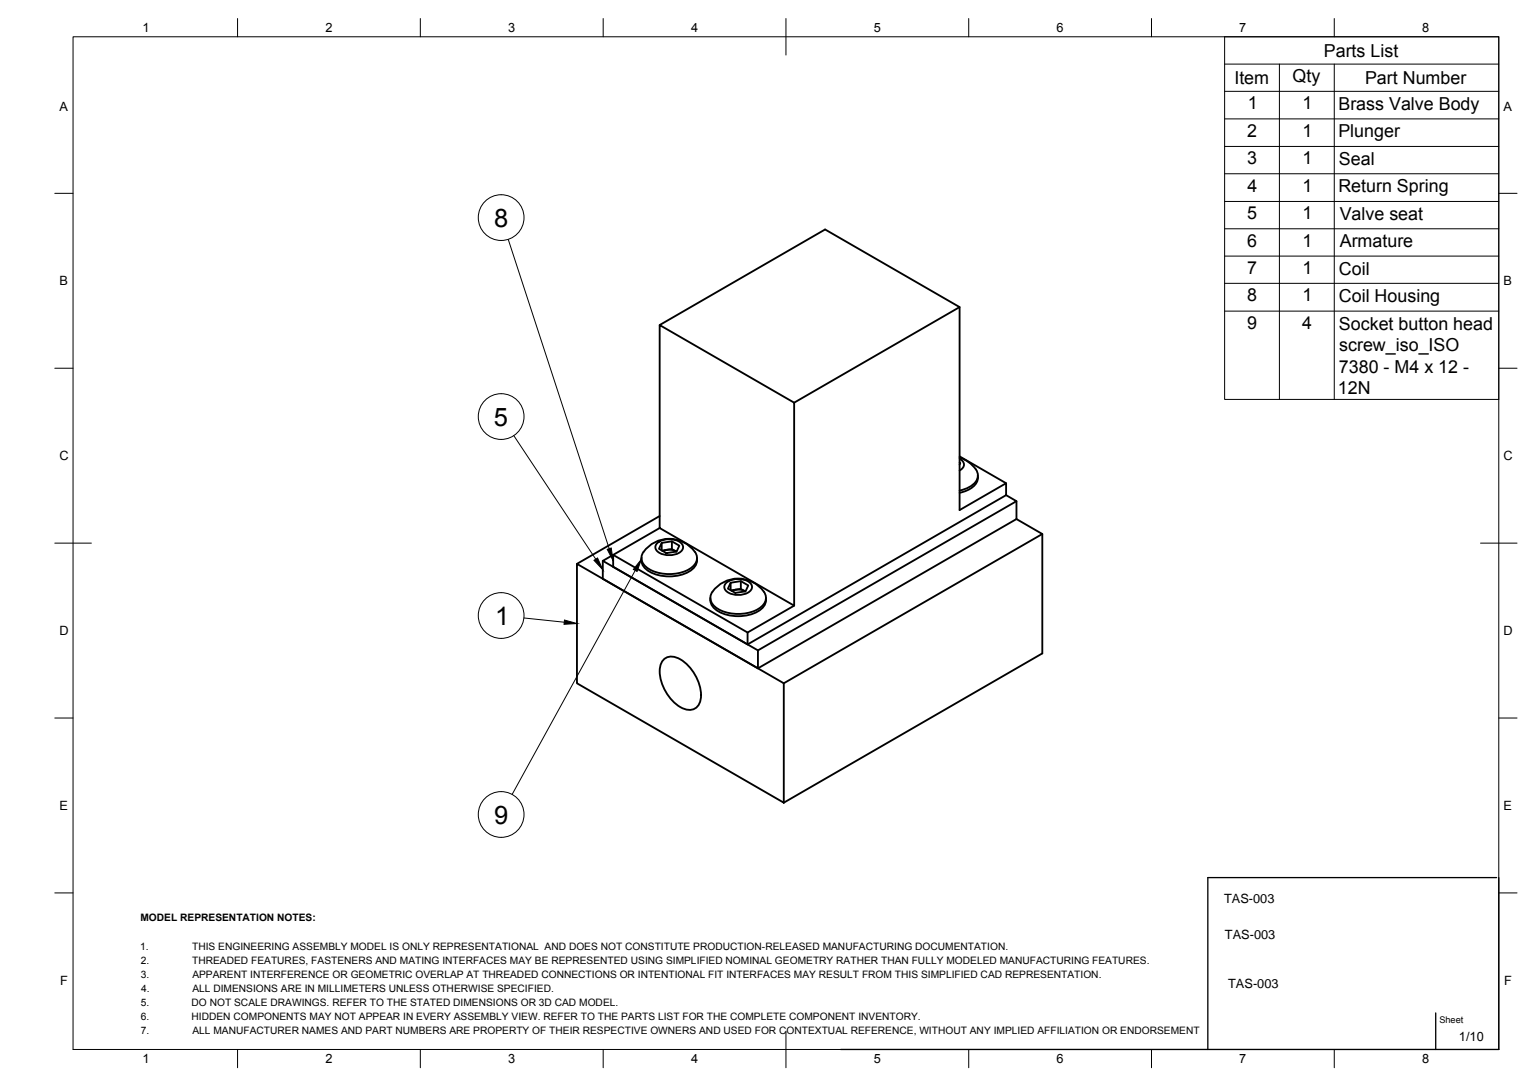
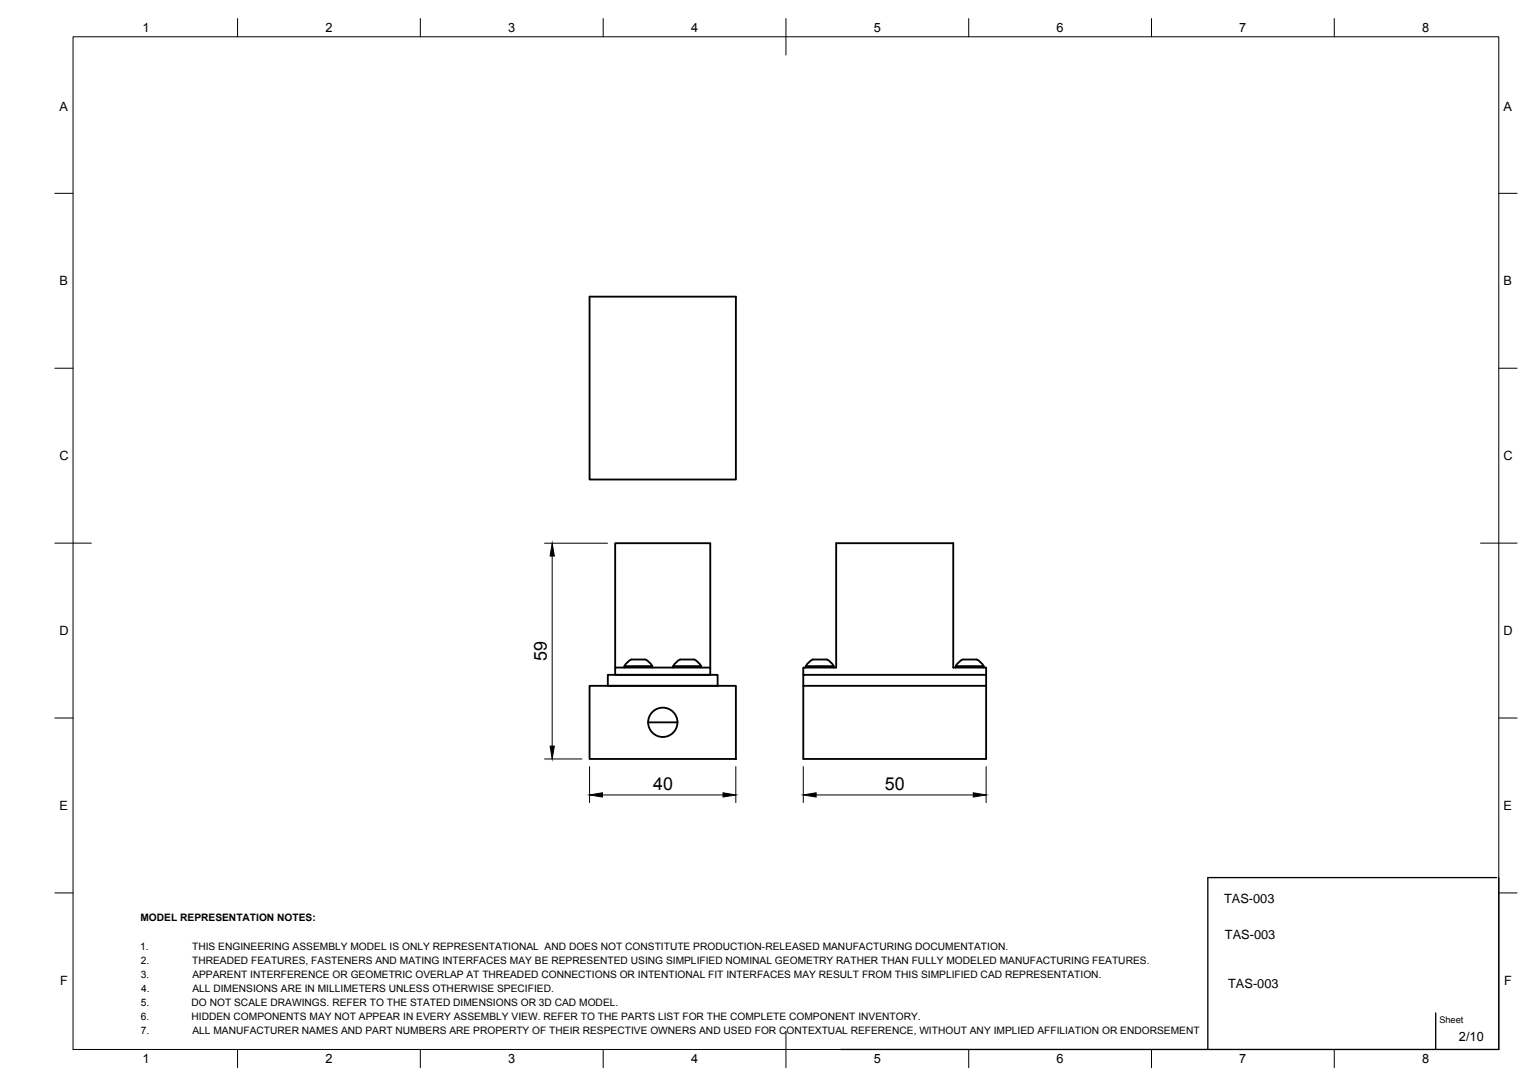
ISO-10303-21;
HEADER;
/* Generated by software containing ST-Developer
 * from STEP Tools, Inc. (www.steptools.com) 
 */

FILE_DESCRIPTION(
/* description */ ('STEP AP214'),
/* implementation_level */ '2;1');

FILE_NAME(
/* name */ 'TAS-003',
/* time_stamp */ '2026-11-04T19:43:37-08:00',
/* author */ (''),
/* organization */ (''),
/* preprocessor_version */ 'ST-DEVELOPER v20.2',
/* originating_system */ 'Autodesk Translation Framework v15.17.0.0',
/* authorisation */ '');

FILE_SCHEMA (('AUTOMOTIVE_DESIGN { 1 0 10303 214 3 1 1 }'));
ENDSEC;

DATA;
#10=MECHANICAL_DESIGN_GEOMETRIC_PRESENTATION_REPRESENTATION('',(#115,#116,
#117,#118,#119,#120,#121,#122,#123,#124,#125,#126,#127,#128,#129,#130,#131,
#132,#133,#134,#135),#7627);
#11=ITEM_DEFINED_TRANSFORMATION($,$,#2535,#2852);
#12=ITEM_DEFINED_TRANSFORMATION($,$,#2572,#2853);
#13=ITEM_DEFINED_TRANSFORMATION($,$,#2590,#2854);
#14=ITEM_DEFINED_TRANSFORMATION($,$,#2600,#2855);
#15=ITEM_DEFINED_TRANSFORMATION($,$,#2608,#2856);
#16=ITEM_DEFINED_TRANSFORMATION($,$,#2630,#2857);
#17=ITEM_DEFINED_TRANSFORMATION($,$,#2645,#2858);
#18=ITEM_DEFINED_TRANSFORMATION($,$,#2776,#2859);
#19=ITEM_DEFINED_TRANSFORMATION($,$,#2816,#2860);
#20=ITEM_DEFINED_TRANSFORMATION($,$,#2816,#2861);
#21=ITEM_DEFINED_TRANSFORMATION($,$,#2816,#2862);
#22=ITEM_DEFINED_TRANSFORMATION($,$,#2816,#2863);
#23=(
REPRESENTATION_RELATIONSHIP($,$,#7665,#7664)
REPRESENTATION_RELATIONSHIP_WITH_TRANSFORMATION(#11)
SHAPE_REPRESENTATION_RELATIONSHIP()
);
#24=(
REPRESENTATION_RELATIONSHIP($,$,#7666,#7664)
REPRESENTATION_RELATIONSHIP_WITH_TRANSFORMATION(#12)
SHAPE_REPRESENTATION_RELATIONSHIP()
);
#25=(
REPRESENTATION_RELATIONSHIP($,$,#7667,#7664)
REPRESENTATION_RELATIONSHIP_WITH_TRANSFORMATION(#13)
SHAPE_REPRESENTATION_RELATIONSHIP()
);
#26=(
REPRESENTATION_RELATIONSHIP($,$,#7668,#7664)
REPRESENTATION_RELATIONSHIP_WITH_TRANSFORMATION(#14)
SHAPE_REPRESENTATION_RELATIONSHIP()
);
#27=(
REPRESENTATION_RELATIONSHIP($,$,#7669,#7664)
REPRESENTATION_RELATIONSHIP_WITH_TRANSFORMATION(#15)
SHAPE_REPRESENTATION_RELATIONSHIP()
);
#28=(
REPRESENTATION_RELATIONSHIP($,$,#7670,#7664)
REPRESENTATION_RELATIONSHIP_WITH_TRANSFORMATION(#16)
SHAPE_REPRESENTATION_RELATIONSHIP()
);
#29=(
REPRESENTATION_RELATIONSHIP($,$,#7671,#7664)
REPRESENTATION_RELATIONSHIP_WITH_TRANSFORMATION(#17)
SHAPE_REPRESENTATION_RELATIONSHIP()
);
#30=(
REPRESENTATION_RELATIONSHIP($,$,#7672,#7664)
REPRESENTATION_RELATIONSHIP_WITH_TRANSFORMATION(#18)
SHAPE_REPRESENTATION_RELATIONSHIP()
);
#31=(
REPRESENTATION_RELATIONSHIP($,$,#7673,#7664)
REPRESENTATION_RELATIONSHIP_WITH_TRANSFORMATION(#19)
SHAPE_REPRESENTATION_RELATIONSHIP()
);
#32=(
REPRESENTATION_RELATIONSHIP($,$,#7673,#7664)
REPRESENTATION_RELATIONSHIP_WITH_TRANSFORMATION(#20)
SHAPE_REPRESENTATION_RELATIONSHIP()
);
#33=(
REPRESENTATION_RELATIONSHIP($,$,#7673,#7664)
REPRESENTATION_RELATIONSHIP_WITH_TRANSFORMATION(#21)
SHAPE_REPRESENTATION_RELATIONSHIP()
);
#34=(
REPRESENTATION_RELATIONSHIP($,$,#7673,#7664)
REPRESENTATION_RELATIONSHIP_WITH_TRANSFORMATION(#22)
SHAPE_REPRESENTATION_RELATIONSHIP()
);
#35=CONTEXT_DEPENDENT_SHAPE_REPRESENTATION(#23,#7652);
#36=CONTEXT_DEPENDENT_SHAPE_REPRESENTATION(#24,#7653);
#37=CONTEXT_DEPENDENT_SHAPE_REPRESENTATION(#25,#7654);
#38=CONTEXT_DEPENDENT_SHAPE_REPRESENTATION(#26,#7655);
#39=CONTEXT_DEPENDENT_SHAPE_REPRESENTATION(#27,#7656);
#40=CONTEXT_DEPENDENT_SHAPE_REPRESENTATION(#28,#7657);
#41=CONTEXT_DEPENDENT_SHAPE_REPRESENTATION(#29,#7658);
#42=CONTEXT_DEPENDENT_SHAPE_REPRESENTATION(#30,#7659);
#43=CONTEXT_DEPENDENT_SHAPE_REPRESENTATION(#31,#7660);
#44=CONTEXT_DEPENDENT_SHAPE_REPRESENTATION(#32,#7661);
#45=CONTEXT_DEPENDENT_SHAPE_REPRESENTATION(#33,#7662);
#46=CONTEXT_DEPENDENT_SHAPE_REPRESENTATION(#34,#7663);
#47=NEXT_ASSEMBLY_USAGE_OCCURRENCE('Brass Valve Body:1',
'Brass Valve Body:1','Brass Valve Body:1',#7675,#7676,
'Brass Valve Body:1');
#48=NEXT_ASSEMBLY_USAGE_OCCURRENCE('Plunger:1','Plunger:1','Plunger:1',
#7675,#7677,'Plunger:1');
#49=NEXT_ASSEMBLY_USAGE_OCCURRENCE('seal:1','seal:1','seal:1',#7675,#7678,
'seal:1');
#50=NEXT_ASSEMBLY_USAGE_OCCURRENCE('Return Spring:1','Return Spring:1',
'Return Spring:1',#7675,#7679,'Return Spring:1');
#51=NEXT_ASSEMBLY_USAGE_OCCURRENCE('valve seat:1','valve seat:1',
'valve seat:1',#7675,#7680,'valve seat:1');
#52=NEXT_ASSEMBLY_USAGE_OCCURRENCE('armature:1','armature:1',
'armature:1',#7675,#7681,'armature:1');
#53=NEXT_ASSEMBLY_USAGE_OCCURRENCE('coil:1','coil:1','coil:1',#7675,#7682,
'coil:1');
#54=NEXT_ASSEMBLY_USAGE_OCCURRENCE('Coil Housing:1','Coil Housing:1',
'Coil Housing:1',#7675,#7683,'Coil Housing:1');
#55=NEXT_ASSEMBLY_USAGE_OCCURRENCE(
'socket button head screw_iso_ISO 7380 - M4 x 12 - 12N:1',
'socket button head screw_iso_ISO 7380 - M4 x 12 - 12N:1',
'socket button head screw_iso_ISO 7380 - M4 x 12 - 12N:1',#7675,#7684,
'socket button head screw_iso_ISO 7380 - M4 x 12 - 12N:1');
#56=NEXT_ASSEMBLY_USAGE_OCCURRENCE(
'socket button head screw_iso_ISO 7380 - M4 x 12 - 12N:2',
'socket button head screw_iso_ISO 7380 - M4 x 12 - 12N:2',
'socket button head screw_iso_ISO 7380 - M4 x 12 - 12N:2',#7675,#7684,
'socket button head screw_iso_ISO 7380 - M4 x 12 - 12N:2');
#57=NEXT_ASSEMBLY_USAGE_OCCURRENCE(
'socket button head screw_iso_ISO 7380 - M4 x 12 - 12N:3',
'socket button head screw_iso_ISO 7380 - M4 x 12 - 12N:3',
'socket button head screw_iso_ISO 7380 - M4 x 12 - 12N:3',#7675,#7684,
'socket button head screw_iso_ISO 7380 - M4 x 12 - 12N:3');
#58=NEXT_ASSEMBLY_USAGE_OCCURRENCE(
'socket button head screw_iso_ISO 7380 - M4 x 12 - 12N:4',
'socket button head screw_iso_ISO 7380 - M4 x 12 - 12N:4',
'socket button head screw_iso_ISO 7380 - M4 x 12 - 12N:4',#7675,#7684,
'socket button head screw_iso_ISO 7380 - M4 x 12 - 12N:4');
#59=SPHERICAL_SURFACE('',#2835,4.3249693283142);
#60=TOROIDAL_SURFACE('',#2646,9.,0.999999999999999);
#61=TOROIDAL_SURFACE('',#2650,9.,0.999999999999999);
#62=TOROIDAL_SURFACE('',#2656,9.,0.999999999999999);
#63=TOROIDAL_SURFACE('',#2660,9.,0.999999999999999);
#64=TOROIDAL_SURFACE('',#2666,9.,0.999999999999999);
#65=TOROIDAL_SURFACE('',#2670,9.,0.999999999999999);
#66=TOROIDAL_SURFACE('',#2676,9.,0.999999999999999);
#67=TOROIDAL_SURFACE('',#2680,9.,0.999999999999999);
#68=TOROIDAL_SURFACE('',#2686,9.,0.999999999999999);
#69=TOROIDAL_SURFACE('',#2690,9.,0.999999999999999);
#70=TOROIDAL_SURFACE('',#2696,9.,0.999999999999999);
#71=TOROIDAL_SURFACE('',#2700,9.,0.999999999999999);
#72=TOROIDAL_SURFACE('',#2706,9.,0.999999999999999);
#73=TOROIDAL_SURFACE('',#2710,9.,0.999999999999999);
#74=TOROIDAL_SURFACE('',#2716,9.,0.999999999999999);
#75=TOROIDAL_SURFACE('',#2720,9.,0.999999999999999);
#76=TOROIDAL_SURFACE('',#2726,9.,0.999999999999999);
#77=TOROIDAL_SURFACE('',#2730,9.,0.999999999999999);
#78=TOROIDAL_SURFACE('',#2736,9.,0.999999999999999);
#79=TOROIDAL_SURFACE('',#2740,9.,0.999999999999999);
#80=TOROIDAL_SURFACE('',#2746,9.,0.999999999999999);
#81=TOROIDAL_SURFACE('',#2750,9.,0.999999999999999);
#82=TOROIDAL_SURFACE('',#2756,9.,0.999999999999999);
#83=TOROIDAL_SURFACE('',#2760,9.,0.999999999999999);
#84=TOROIDAL_SURFACE('',#2766,9.,0.999999999999999);
#85=TOROIDAL_SURFACE('',#2770,9.,0.999999999999999);
#86=TOROIDAL_SURFACE('',#2777,2.2,0.2);
#87=TOROIDAL_SURFACE('',#2781,2.2,0.2);
#88=TOROIDAL_SURFACE('',#2785,2.2,0.2);
#89=TOROIDAL_SURFACE('',#2789,2.2,0.2);
#90=TOROIDAL_SURFACE('',#2824,2.2,0.2);
#91=(
BOUNDED_CURVE()
B_SPLINE_CURVE(2,(#5252,#5253,#5254,#5255,#5256,#5257,#5258,#5259,#5260,
#5261,#5262,#5263,#5264,#5265,#5266,#5267,#5268,#5269,#5270,#5271,#5272,
#5273,#5274,#5275,#5276,#5277,#5278,#5279,#5280,#5281,#5282,#5283,#5284,
#5285,#5286,#5287,#5288,#5289,#5290,#5291,#5292,#5293,#5294,#5295,#5296,
#5297,#5298,#5299,#5300,#5301,#5302,#5303,#5304,#5305,#5306,#5307,#5308,
#5309,#5310,#5311,#5312,#5313,#5314,#5315,#5316,#5317,#5318,#5319,#5320,
#5321,#5322,#5323,#5324,#5325,#5326,#5327,#5328,#5329,#5330,#5331,#5332,
#5333,#5334,#5335,#5336,#5337,#5338,#5339,#5340,#5341,#5342,#5343,#5344,
#5345,#5346,#5347,#5348,#5349,#5350,#5351,#5352,#5353,#5354,#5355,#5356,
#5357,#5358,#5359,#5360,#5361,#5362,#5363,#5364,#5365,#5366,#5367,#5368,
#5369,#5370,#5371,#5372,#5373,#5374,#5375,#5376,#5377,#5378,#5379,#5380,
#5381,#5382,#5383,#5384,#5385,#5386,#5387,#5388,#5389,#5390,#5391,#5392,
#5393,#5394,#5395,#5396,#5397,#5398,#5399,#5400,#5401,#5402,#5403,#5404,
#5405,#5406,#5407,#5408,#5409,#5410,#5411,#5412,#5413,#5414,#5415,#5416,
#5417,#5418,#5419,#5420,#5421,#5422,#5423,#5424,#5425,#5426,#5427,#5428,
#5429,#5430,#5431,#5432,#5433,#5434,#5435,#5436,#5437,#5438,#5439,#5440,
#5441,#5442,#5443,#5444,#5445,#5446,#5447,#5448,#5449,#5450),
 .UNSPECIFIED.,.F.,.F.)
B_SPLINE_CURVE_WITH_KNOTS((3,2,2,2,2,2,2,2,2,2,2,2,2,2,2,2,2,2,2,2,2,2,
2,2,2,2,2,2,2,2,2,2,2,2,2,2,2,2,2,2,2,2,2,2,2,2,2,2,2,2,2,2,2,2,2,2,2,2,
2,2,2,2,2,2,2,2,2,2,2,2,2,2,2,2,2,2,2,2,2,2,2,2,2,2,2,2,2,2,2,2,2,2,2,2,
2,2,2,2,2,3),(0.0198656835159411,0.02,0.03,0.04,0.05,0.06,0.07,0.08,0.09,
0.1,0.11,0.12,0.13,0.14,0.15,0.16,0.17,0.18,0.19,0.2,0.21,0.22,0.23,0.24,
0.25,0.26,0.27,0.28,0.29,0.3,0.31,0.32,0.33,0.34,0.35,0.36,0.37,0.38,0.39,
0.4,0.41,0.42,0.43,0.44,0.45,0.46,0.47,0.48,0.49,0.5,0.51,0.52,0.53,0.54,
0.55,0.56,0.57,0.58,0.59,0.6,0.61,0.62,0.63,0.64,0.65,0.66,0.67,0.68,0.69,
0.7,0.71,0.72,0.73,0.74,0.75,0.76,0.77,0.78,0.79,0.8,0.81,0.82,0.83,0.84,
0.85,0.86,0.87,0.88,0.89,0.9,0.91,0.92,0.93,0.94,0.95,0.96,0.97,0.98,0.99,
1.),.UNSPECIFIED.)
CURVE()
GEOMETRIC_REPRESENTATION_ITEM()
RATIONAL_B_SPLINE_CURVE((0.998702876377649,0.999342608335117,1.,0.951056516295154,
1.,0.951056516295154,1.,0.951056516295154,1.,0.951056516295154,1.,0.951056516295154,
1.,0.951056516295154,1.,0.951056516295154,1.,0.951056516295154,1.,0.951056516295154,
1.,0.951056516295154,1.,0.951056516295154,1.,0.951056516295154,1.,0.951056516295154,
1.,0.951056516295154,1.,0.951056516295154,1.,0.951056516295154,1.,0.951056516295154,
1.,0.951056516295154,1.,0.951056516295154,1.,0.951056516295154,1.,0.951056516295154,
1.,0.951056516295154,1.,0.951056516295154,1.,0.951056516295154,1.,0.951056516295154,
1.,0.951056516295154,1.,0.951056516295154,1.,0.951056516295154,1.,0.951056516295154,
1.,0.951056516295154,1.,0.951056516295154,1.,0.951056516295154,1.,0.951056516295154,
1.,0.951056516295154,1.,0.951056516295154,1.,0.951056516295154,1.,0.951056516295154,
1.,0.951056516295154,1.,0.951056516295154,1.,0.951056516295154,1.,0.951056516295154,
1.,0.951056516295154,1.,0.951056516295154,1.,0.951056516295154,1.,0.951056516295154,
1.,0.951056516295154,1.,0.951056516295154,1.,0.951056516295154,1.,0.951056516295154,
1.,0.951056516295154,1.,0.951056516295154,1.,0.951056516295154,1.,0.951056516295154,
1.,0.951056516295154,1.,0.951056516295154,1.,0.951056516295154,1.,0.951056516295154,
1.,0.951056516295154,1.,0.951056516295154,1.,0.951056516295154,1.,0.951056516295154,
1.,0.951056516295154,1.,0.951056516295154,1.,0.951056516295154,1.,0.951056516295154,
1.,0.951056516295154,1.,0.951056516295154,1.,0.951056516295154,1.,0.951056516295154,
1.,0.951056516295154,1.,0.951056516295154,1.,0.951056516295154,1.,0.951056516295154,
1.,0.951056516295154,1.,0.951056516295154,1.,0.951056516295154,1.,0.951056516295154,
1.,0.951056516295154,1.,0.951056516295154,1.,0.951056516295154,1.,0.951056516295154,
1.,0.951056516295154,1.,0.951056516295154,1.,0.951056516295154,1.,0.951056516295154,
1.,0.951056516295154,1.,0.951056516295154,1.,0.951056516295154,1.,0.951056516295154,
1.,0.951056516295154,1.,0.951056516295154,1.,0.951056516295154,1.,0.951056516295154,
1.,0.951056516295154,1.,0.951056516295154,1.,0.951056516295154,1.,0.951056516295154,
1.,0.951056516295154,1.))
REPRESENTATION_ITEM('')
);
#92=(
BOUNDED_CURVE()
B_SPLINE_CURVE(2,(#5454,#5455,#5456,#5457,#5458,#5459,#5460,#5461,#5462,
#5463,#5464,#5465,#5466,#5467,#5468,#5469,#5470,#5471,#5472,#5473,#5474,
#5475,#5476,#5477,#5478,#5479,#5480,#5481,#5482,#5483,#5484,#5485,#5486,
#5487,#5488,#5489,#5490,#5491,#5492,#5493,#5494,#5495,#5496,#5497,#5498,
#5499,#5500,#5501,#5502,#5503,#5504,#5505,#5506,#5507,#5508,#5509,#5510,
#5511,#5512,#5513,#5514,#5515,#5516,#5517,#5518,#5519,#5520,#5521,#5522,
#5523,#5524,#5525,#5526,#5527,#5528,#5529,#5530,#5531,#5532,#5533,#5534,
#5535,#5536,#5537,#5538,#5539,#5540,#5541,#5542,#5543,#5544,#5545,#5546,
#5547,#5548,#5549,#5550,#5551,#5552,#5553,#5554,#5555,#5556,#5557,#5558,
#5559,#5560,#5561,#5562,#5563,#5564,#5565,#5566,#5567,#5568,#5569,#5570,
#5571,#5572,#5573,#5574,#5575,#5576,#5577,#5578,#5579,#5580,#5581,#5582,
#5583,#5584,#5585,#5586,#5587,#5588,#5589,#5590,#5591,#5592,#5593,#5594,
#5595,#5596,#5597,#5598,#5599,#5600,#5601,#5602,#5603,#5604,#5605,#5606,
#5607,#5608,#5609,#5610,#5611,#5612,#5613,#5614,#5615,#5616,#5617,#5618,
#5619,#5620,#5621,#5622,#5623,#5624,#5625,#5626,#5627,#5628,#5629,#5630,
#5631,#5632,#5633,#5634,#5635,#5636,#5637,#5638,#5639,#5640,#5641,#5642,
#5643,#5644,#5645,#5646,#5647,#5648,#5649,#5650,#5651,#5652,#5653,#5654),
 .UNSPECIFIED.,.F.,.F.)
B_SPLINE_CURVE_WITH_KNOTS((3,2,2,2,2,2,2,2,2,2,2,2,2,2,2,2,2,2,2,2,2,2,
2,2,2,2,2,2,2,2,2,2,2,2,2,2,2,2,2,2,2,2,2,2,2,2,2,2,2,2,2,2,2,2,2,2,2,2,
2,2,2,2,2,2,2,2,2,2,2,2,2,2,2,2,2,2,2,2,2,2,2,2,2,2,2,2,2,2,2,2,2,2,2,2,
2,2,2,2,2,2,3),(0.,0.01,0.02,0.03,0.04,0.05,0.06,0.07,0.08,0.09,0.1,0.11,
0.12,0.13,0.14,0.15,0.16,0.17,0.18,0.19,0.2,0.21,0.22,0.23,0.24,0.25,0.26,
0.27,0.28,0.29,0.3,0.31,0.32,0.33,0.34,0.35,0.36,0.37,0.38,0.39,0.4,0.41,
0.42,0.43,0.44,0.45,0.46,0.47,0.48,0.49,0.5,0.51,0.52,0.53,0.54,0.55,0.56,
0.57,0.58,0.59,0.6,0.61,0.62,0.63,0.64,0.65,0.66,0.67,0.68,0.69,0.7,0.71,
0.72,0.73,0.74,0.75,0.76,0.77,0.78,0.79,0.8,0.81,0.82,0.83,0.84,0.85,0.86,
0.87,0.88,0.89,0.9,0.91,0.92,0.93,0.94,0.95,0.96,0.97,0.98,0.99,1.),
 .UNSPECIFIED.)
CURVE()
GEOMETRIC_REPRESENTATION_ITEM()
RATIONAL_B_SPLINE_CURVE((1.,0.951056516295154,1.,0.951056516295154,1.,0.951056516295154,
1.,0.951056516295154,1.,0.951056516295154,1.,0.951056516295154,1.,0.951056516295154,
1.,0.951056516295154,1.,0.951056516295154,1.,0.951056516295154,1.,0.951056516295154,
1.,0.951056516295154,1.,0.951056516295154,1.,0.951056516295154,1.,0.951056516295154,
1.,0.951056516295154,1.,0.951056516295154,1.,0.951056516295154,1.,0.951056516295154,
1.,0.951056516295154,1.,0.951056516295154,1.,0.951056516295154,1.,0.951056516295154,
1.,0.951056516295154,1.,0.951056516295154,1.,0.951056516295154,1.,0.951056516295154,
1.,0.951056516295154,1.,0.951056516295154,1.,0.951056516295154,1.,0.951056516295154,
1.,0.951056516295154,1.,0.951056516295154,1.,0.951056516295154,1.,0.951056516295154,
1.,0.951056516295154,1.,0.951056516295154,1.,0.951056516295154,1.,0.951056516295154,
1.,0.951056516295154,1.,0.951056516295154,1.,0.951056516295154,1.,0.951056516295154,
1.,0.951056516295154,1.,0.951056516295154,1.,0.951056516295154,1.,0.951056516295154,
1.,0.951056516295154,1.,0.951056516295154,1.,0.951056516295154,1.,0.951056516295154,
1.,0.951056516295154,1.,0.951056516295154,1.,0.951056516295154,1.,0.951056516295154,
1.,0.951056516295154,1.,0.951056516295154,1.,0.951056516295154,1.,0.951056516295154,
1.,0.951056516295154,1.,0.951056516295154,1.,0.951056516295154,1.,0.951056516295154,
1.,0.951056516295154,1.,0.951056516295154,1.,0.951056516295154,1.,0.951056516295154,
1.,0.951056516295154,1.,0.951056516295154,1.,0.951056516295154,1.,0.951056516295154,
1.,0.951056516295154,1.,0.951056516295154,1.,0.951056516295154,1.,0.951056516295154,
1.,0.951056516295154,1.,0.951056516295154,1.,0.951056516295154,1.,0.951056516295154,
1.,0.951056516295154,1.,0.951056516295154,1.,0.951056516295154,1.,0.951056516295154,
1.,0.951056516295154,1.,0.951056516295154,1.,0.951056516295154,1.,0.951056516295154,
1.,0.951056516295154,1.,0.951056516295154,1.,0.951056516295154,1.,0.951056516295154,
1.,0.951056516295154,1.,0.951056516295154,1.,0.951056516295154,1.,0.951056516295154,
1.,0.951056516295154,1.,0.951056516295154,1.,0.951056516295154,1.,0.951056516295154,
1.,0.951056516295154,1.))
REPRESENTATION_ITEM('')
);
#93=B_SPLINE_CURVE_WITH_KNOTS('',3,(#5233,#5234,#5235,#5236,#5237,#5238,
#5239,#5240,#5241,#5242,#5243,#5244,#5245,#5246,#5247,#5248,#5249,#5250),
 .UNSPECIFIED.,.F.,.F.,(4,2,2,2,2,2,2,2,4),(1.00001181076875E-6,0.00157652680691075,
0.00330831465659758,0.00743558655671621,0.0176553842502255,0.0434588790338826,
0.0717527150596022,0.0885002828939342,0.104340792550165),.UNSPECIFIED.);
#94=B_SPLINE_CURVE_WITH_KNOTS('',3,(#7069,#7070,#7071,#7072,#7073,#7074,
#7075,#7076,#7077,#7078,#7079,#7080,#7081,#7082,#7083,#7084,#7085,#7086),
 .UNSPECIFIED.,.F.,.F.,(4,2,2,2,2,2,2,2,4),(0.,0.132188814767311,0.250674887289718,
0.391272166110131,0.552836235371939,0.655950520994649,0.689957274574409,
0.701859173270786,0.711834218003037),.UNSPECIFIED.);
#95=(
BOUNDED_SURFACE()
B_SPLINE_SURFACE(3,2,((#3824,#3825,#3826,#3827,#3828,#3829,#3830,#3831,
#3832,#3833,#3834,#3835,#3836,#3837,#3838,#3839,#3840,#3841,#3842,#3843,
#3844,#3845,#3846,#3847,#3848,#3849,#3850,#3851,#3852,#3853,#3854,#3855,
#3856,#3857,#3858,#3859,#3860,#3861,#3862,#3863,#3864,#3865,#3866,#3867,
#3868,#3869,#3870,#3871,#3872,#3873,#3874,#3875,#3876,#3877,#3878,#3879,
#3880,#3881,#3882,#3883,#3884,#3885,#3886,#3887,#3888,#3889,#3890,#3891,
#3892,#3893,#3894,#3895,#3896,#3897,#3898,#3899,#3900,#3901,#3902,#3903,
#3904,#3905,#3906,#3907,#3908,#3909,#3910,#3911,#3912,#3913,#3914,#3915,
#3916,#3917,#3918,#3919,#3920,#3921,#3922,#3923,#3924,#3925,#3926,#3927,
#3928,#3929,#3930,#3931,#3932,#3933,#3934,#3935,#3936,#3937,#3938,#3939,
#3940,#3941,#3942,#3943,#3944,#3945,#3946,#3947,#3948,#3949,#3950,#3951,
#3952,#3953,#3954,#3955,#3956,#3957,#3958,#3959,#3960,#3961,#3962,#3963,
#3964,#3965,#3966,#3967,#3968,#3969,#3970,#3971,#3972,#3973,#3974,#3975,
#3976,#3977,#3978,#3979,#3980,#3981,#3982,#3983,#3984,#3985,#3986,#3987,
#3988,#3989,#3990,#3991,#3992,#3993,#3994,#3995,#3996,#3997,#3998,#3999,
#4000,#4001,#4002,#4003,#4004,#4005,#4006,#4007,#4008,#4009,#4010,#4011,
#4012,#4013,#4014,#4015,#4016,#4017,#4018,#4019,#4020,#4021,#4022,#4023,
#4024),(#4025,#4026,#4027,#4028,#4029,#4030,#4031,#4032,#4033,#4034,#4035,
#4036,#4037,#4038,#4039,#4040,#4041,#4042,#4043,#4044,#4045,#4046,#4047,
#4048,#4049,#4050,#4051,#4052,#4053,#4054,#4055,#4056,#4057,#4058,#4059,
#4060,#4061,#4062,#4063,#4064,#4065,#4066,#4067,#4068,#4069,#4070,#4071,
#4072,#4073,#4074,#4075,#4076,#4077,#4078,#4079,#4080,#4081,#4082,#4083,
#4084,#4085,#4086,#4087,#4088,#4089,#4090,#4091,#4092,#4093,#4094,#4095,
#4096,#4097,#4098,#4099,#4100,#4101,#4102,#4103,#4104,#4105,#4106,#4107,
#4108,#4109,#4110,#4111,#4112,#4113,#4114,#4115,#4116,#4117,#4118,#4119,
#4120,#4121,#4122,#4123,#4124,#4125,#4126,#4127,#4128,#4129,#4130,#4131,
#4132,#4133,#4134,#4135,#4136,#4137,#4138,#4139,#4140,#4141,#4142,#4143,
#4144,#4145,#4146,#4147,#4148,#4149,#4150,#4151,#4152,#4153,#4154,#4155,
#4156,#4157,#4158,#4159,#4160,#4161,#4162,#4163,#4164,#4165,#4166,#4167,
#4168,#4169,#4170,#4171,#4172,#4173,#4174,#4175,#4176,#4177,#4178,#4179,
#4180,#4181,#4182,#4183,#4184,#4185,#4186,#4187,#4188,#4189,#4190,#4191,
#4192,#4193,#4194,#4195,#4196,#4197,#4198,#4199,#4200,#4201,#4202,#4203,
#4204,#4205,#4206,#4207,#4208,#4209,#4210,#4211,#4212,#4213,#4214,#4215,
#4216,#4217,#4218,#4219,#4220,#4221,#4222,#4223,#4224,#4225),(#4226,#4227,
#4228,#4229,#4230,#4231,#4232,#4233,#4234,#4235,#4236,#4237,#4238,#4239,
#4240,#4241,#4242,#4243,#4244,#4245,#4246,#4247,#4248,#4249,#4250,#4251,
#4252,#4253,#4254,#4255,#4256,#4257,#4258,#4259,#4260,#4261,#4262,#4263,
#4264,#4265,#4266,#4267,#4268,#4269,#4270,#4271,#4272,#4273,#4274,#4275,
#4276,#4277,#4278,#4279,#4280,#4281,#4282,#4283,#4284,#4285,#4286,#4287,
#4288,#4289,#4290,#4291,#4292,#4293,#4294,#4295,#4296,#4297,#4298,#4299,
#4300,#4301,#4302,#4303,#4304,#4305,#4306,#4307,#4308,#4309,#4310,#4311,
#4312,#4313,#4314,#4315,#4316,#4317,#4318,#4319,#4320,#4321,#4322,#4323,
#4324,#4325,#4326,#4327,#4328,#4329,#4330,#4331,#4332,#4333,#4334,#4335,
#4336,#4337,#4338,#4339,#4340,#4341,#4342,#4343,#4344,#4345,#4346,#4347,
#4348,#4349,#4350,#4351,#4352,#4353,#4354,#4355,#4356,#4357,#4358,#4359,
#4360,#4361,#4362,#4363,#4364,#4365,#4366,#4367,#4368,#4369,#4370,#4371,
#4372,#4373,#4374,#4375,#4376,#4377,#4378,#4379,#4380,#4381,#4382,#4383,
#4384,#4385,#4386,#4387,#4388,#4389,#4390,#4391,#4392,#4393,#4394,#4395,
#4396,#4397,#4398,#4399,#4400,#4401,#4402,#4403,#4404,#4405,#4406,#4407,
#4408,#4409,#4410,#4411,#4412,#4413,#4414,#4415,#4416,#4417,#4418,#4419,
#4420,#4421,#4422,#4423,#4424,#4425,#4426),(#4427,#4428,#4429,#4430,#4431,
#4432,#4433,#4434,#4435,#4436,#4437,#4438,#4439,#4440,#4441,#4442,#4443,
#4444,#4445,#4446,#4447,#4448,#4449,#4450,#4451,#4452,#4453,#4454,#4455,
#4456,#4457,#4458,#4459,#4460,#4461,#4462,#4463,#4464,#4465,#4466,#4467,
#4468,#4469,#4470,#4471,#4472,#4473,#4474,#4475,#4476,#4477,#4478,#4479,
#4480,#4481,#4482,#4483,#4484,#4485,#4486,#4487,#4488,#4489,#4490,#4491,
#4492,#4493,#4494,#4495,#4496,#4497,#4498,#4499,#4500,#4501,#4502,#4503,
#4504,#4505,#4506,#4507,#4508,#4509,#4510,#4511,#4512,#4513,#4514,#4515,
#4516,#4517,#4518,#4519,#4520,#4521,#4522,#4523,#4524,#4525,#4526,#4527,
#4528,#4529,#4530,#4531,#4532,#4533,#4534,#4535,#4536,#4537,#4538,#4539,
#4540,#4541,#4542,#4543,#4544,#4545,#4546,#4547,#4548,#4549,#4550,#4551,
#4552,#4553,#4554,#4555,#4556,#4557,#4558,#4559,#4560,#4561,#4562,#4563,
#4564,#4565,#4566,#4567,#4568,#4569,#4570,#4571,#4572,#4573,#4574,#4575,
#4576,#4577,#4578,#4579,#4580,#4581,#4582,#4583,#4584,#4585,#4586,#4587,
#4588,#4589,#4590,#4591,#4592,#4593,#4594,#4595,#4596,#4597,#4598,#4599,
#4600,#4601,#4602,#4603,#4604,#4605,#4606,#4607,#4608,#4609,#4610,#4611,
#4612,#4613,#4614,#4615,#4616,#4617,#4618,#4619,#4620,#4621,#4622,#4623,
#4624,#4625,#4626,#4627),(#4628,#4629,#4630,#4631,#4632,#4633,#4634,#4635,
#4636,#4637,#4638,#4639,#4640,#4641,#4642,#4643,#4644,#4645,#4646,#4647,
#4648,#4649,#4650,#4651,#4652,#4653,#4654,#4655,#4656,#4657,#4658,#4659,
#4660,#4661,#4662,#4663,#4664,#4665,#4666,#4667,#4668,#4669,#4670,#4671,
#4672,#4673,#4674,#4675,#4676,#4677,#4678,#4679,#4680,#4681,#4682,#4683,
#4684,#4685,#4686,#4687,#4688,#4689,#4690,#4691,#4692,#4693,#4694,#4695,
#4696,#4697,#4698,#4699,#4700,#4701,#4702,#4703,#4704,#4705,#4706,#4707,
#4708,#4709,#4710,#4711,#4712,#4713,#4714,#4715,#4716,#4717,#4718,#4719,
#4720,#4721,#4722,#4723,#4724,#4725,#4726,#4727,#4728,#4729,#4730,#4731,
#4732,#4733,#4734,#4735,#4736,#4737,#4738,#4739,#4740,#4741,#4742,#4743,
#4744,#4745,#4746,#4747,#4748,#4749,#4750,#4751,#4752,#4753,#4754,#4755,
#4756,#4757,#4758,#4759,#4760,#4761,#4762,#4763,#4764,#4765,#4766,#4767,
#4768,#4769,#4770,#4771,#4772,#4773,#4774,#4775,#4776,#4777,#4778,#4779,
#4780,#4781,#4782,#4783,#4784,#4785,#4786,#4787,#4788,#4789,#4790,#4791,
#4792,#4793,#4794,#4795,#4796,#4797,#4798,#4799,#4800,#4801,#4802,#4803,
#4804,#4805,#4806,#4807,#4808,#4809,#4810,#4811,#4812,#4813,#4814,#4815,
#4816,#4817,#4818,#4819,#4820,#4821,#4822,#4823,#4824,#4825,#4826,#4827,
#4828),(#4829,#4830,#4831,#4832,#4833,#4834,#4835,#4836,#4837,#4838,#4839,
#4840,#4841,#4842,#4843,#4844,#4845,#4846,#4847,#4848,#4849,#4850,#4851,
#4852,#4853,#4854,#4855,#4856,#4857,#4858,#4859,#4860,#4861,#4862,#4863,
#4864,#4865,#4866,#4867,#4868,#4869,#4870,#4871,#4872,#4873,#4874,#4875,
#4876,#4877,#4878,#4879,#4880,#4881,#4882,#4883,#4884,#4885,#4886,#4887,
#4888,#4889,#4890,#4891,#4892,#4893,#4894,#4895,#4896,#4897,#4898,#4899,
#4900,#4901,#4902,#4903,#4904,#4905,#4906,#4907,#4908,#4909,#4910,#4911,
#4912,#4913,#4914,#4915,#4916,#4917,#4918,#4919,#4920,#4921,#4922,#4923,
#4924,#4925,#4926,#4927,#4928,#4929,#4930,#4931,#4932,#4933,#4934,#4935,
#4936,#4937,#4938,#4939,#4940,#4941,#4942,#4943,#4944,#4945,#4946,#4947,
#4948,#4949,#4950,#4951,#4952,#4953,#4954,#4955,#4956,#4957,#4958,#4959,
#4960,#4961,#4962,#4963,#4964,#4965,#4966,#4967,#4968,#4969,#4970,#4971,
#4972,#4973,#4974,#4975,#4976,#4977,#4978,#4979,#4980,#4981,#4982,#4983,
#4984,#4985,#4986,#4987,#4988,#4989,#4990,#4991,#4992,#4993,#4994,#4995,
#4996,#4997,#4998,#4999,#5000,#5001,#5002,#5003,#5004,#5005,#5006,#5007,
#5008,#5009,#5010,#5011,#5012,#5013,#5014,#5015,#5016,#5017,#5018,#5019,
#5020,#5021,#5022,#5023,#5024,#5025,#5026,#5027,#5028,#5029),(#5030,#5031,
#5032,#5033,#5034,#5035,#5036,#5037,#5038,#5039,#5040,#5041,#5042,#5043,
#5044,#5045,#5046,#5047,#5048,#5049,#5050,#5051,#5052,#5053,#5054,#5055,
#5056,#5057,#5058,#5059,#5060,#5061,#5062,#5063,#5064,#5065,#5066,#5067,
#5068,#5069,#5070,#5071,#5072,#5073,#5074,#5075,#5076,#5077,#5078,#5079,
#5080,#5081,#5082,#5083,#5084,#5085,#5086,#5087,#5088,#5089,#5090,#5091,
#5092,#5093,#5094,#5095,#5096,#5097,#5098,#5099,#5100,#5101,#5102,#5103,
#5104,#5105,#5106,#5107,#5108,#5109,#5110,#5111,#5112,#5113,#5114,#5115,
#5116,#5117,#5118,#5119,#5120,#5121,#5122,#5123,#5124,#5125,#5126,#5127,
#5128,#5129,#5130,#5131,#5132,#5133,#5134,#5135,#5136,#5137,#5138,#5139,
#5140,#5141,#5142,#5143,#5144,#5145,#5146,#5147,#5148,#5149,#5150,#5151,
#5152,#5153,#5154,#5155,#5156,#5157,#5158,#5159,#5160,#5161,#5162,#5163,
#5164,#5165,#5166,#5167,#5168,#5169,#5170,#5171,#5172,#5173,#5174,#5175,
#5176,#5177,#5178,#5179,#5180,#5181,#5182,#5183,#5184,#5185,#5186,#5187,
#5188,#5189,#5190,#5191,#5192,#5193,#5194,#5195,#5196,#5197,#5198,#5199,
#5200,#5201,#5202,#5203,#5204,#5205,#5206,#5207,#5208,#5209,#5210,#5211,
#5212,#5213,#5214,#5215,#5216,#5217,#5218,#5219,#5220,#5221,#5222,#5223,
#5224,#5225,#5226,#5227,#5228,#5229,#5230)),.UNSPECIFIED.,.T.,.F.,.F.)
B_SPLINE_SURFACE_WITH_KNOTS((4,3,4),(3,2,2,2,2,2,2,2,2,2,2,2,2,2,2,2,2,
2,2,2,2,2,2,2,2,2,2,2,2,2,2,2,2,2,2,2,2,2,2,2,2,2,2,2,2,2,2,2,2,2,2,2,2,
2,2,2,2,2,2,2,2,2,2,2,2,2,2,2,2,2,2,2,2,2,2,2,2,2,2,2,2,2,2,2,2,2,2,2,2,
2,2,2,2,2,2,2,2,2,2,2,3),(0.,0.5,1.),(0.,0.01,0.02,0.03,0.04,0.05,0.06,
0.07,0.08,0.09,0.1,0.11,0.12,0.13,0.14,0.15,0.16,0.17,0.18,0.19,0.2,0.21,
0.22,0.23,0.24,0.25,0.26,0.27,0.28,0.29,0.3,0.31,0.32,0.33,0.34,0.35,0.36,
0.37,0.38,0.39,0.4,0.41,0.42,0.43,0.44,0.45,0.46,0.47,0.48,0.49,0.5,0.51,
0.52,0.53,0.54,0.55,0.56,0.57,0.58,0.59,0.6,0.61,0.62,0.63,0.64,0.65,0.66,
0.67,0.68,0.69,0.7,0.71,0.72,0.73,0.74,0.75,0.76,0.77,0.78,0.79,0.8,0.81,
0.82,0.83,0.84,0.85,0.86,0.87,0.88,0.89,0.9,0.91,0.92,0.93,0.94,0.95,0.96,
0.97,0.98,0.99,1.),.UNSPECIFIED.)
GEOMETRIC_REPRESENTATION_ITEM()
RATIONAL_B_SPLINE_SURFACE(((1.,0.951056516295154,1.,0.951056516295154,1.,
0.951056516295154,1.,0.951056516295154,1.,0.951056516295154,1.,0.951056516295154,
1.,0.951056516295154,1.,0.951056516295154,1.,0.951056516295154,1.,0.951056516295154,
1.,0.951056516295154,1.,0.951056516295154,1.,0.951056516295154,1.,0.951056516295154,
1.,0.951056516295154,1.,0.951056516295154,1.,0.951056516295154,1.,0.951056516295154,
1.,0.951056516295154,1.,0.951056516295154,1.,0.951056516295154,1.,0.951056516295154,
1.,0.951056516295154,1.,0.951056516295154,1.,0.951056516295154,1.,0.951056516295154,
1.,0.951056516295154,1.,0.951056516295154,1.,0.951056516295154,1.,0.951056516295154,
1.,0.951056516295154,1.,0.951056516295154,1.,0.951056516295154,1.,0.951056516295154,
1.,0.951056516295154,1.,0.951056516295154,1.,0.951056516295154,1.,0.951056516295154,
1.,0.951056516295154,1.,0.951056516295154,1.,0.951056516295154,1.,0.951056516295154,
1.,0.951056516295154,1.,0.951056516295154,1.,0.951056516295154,1.,0.951056516295154,
1.,0.951056516295154,1.,0.951056516295154,1.,0.951056516295154,1.,0.951056516295154,
1.,0.951056516295154,1.,0.951056516295154,1.,0.951056516295154,1.,0.951056516295154,
1.,0.951056516295154,1.,0.951056516295154,1.,0.951056516295154,1.,0.951056516295154,
1.,0.951056516295154,1.,0.951056516295154,1.,0.951056516295154,1.,0.951056516295154,
1.,0.951056516295154,1.,0.951056516295154,1.,0.951056516295154,1.,0.951056516295154,
1.,0.951056516295154,1.,0.951056516295154,1.,0.951056516295154,1.,0.951056516295154,
1.,0.951056516295154,1.,0.951056516295154,1.,0.951056516295154,1.,0.951056516295154,
1.,0.951056516295154,1.,0.951056516295154,1.,0.951056516295154,1.,0.951056516295154,
1.,0.951056516295154,1.,0.951056516295154,1.,0.951056516295154,1.,0.951056516295154,
1.,0.951056516295154,1.,0.951056516295154,1.,0.951056516295154,1.,0.951056516295154,
1.,0.951056516295154,1.,0.951056516295154,1.,0.951056516295154,1.,0.951056516295154,
1.,0.951056516295154,1.,0.951056516295154,1.,0.951056516295154,1.,0.951056516295154,
1.,0.951056516295154,1.,0.951056516295154,1.,0.951056516295154,1.,0.951056516295154,
1.,0.951056516295154,1.,0.951056516295154,1.),(0.333333333333333,0.317018838765051,
0.333333333333333,0.317018838765051,0.333333333333333,0.317018838765051,
0.333333333333333,0.317018838765051,0.333333333333333,0.317018838765051,
0.333333333333333,0.317018838765051,0.333333333333333,0.317018838765051,
0.333333333333333,0.317018838765051,0.333333333333333,0.317018838765051,
0.333333333333333,0.317018838765051,0.333333333333333,0.317018838765051,
0.333333333333333,0.317018838765051,0.333333333333333,0.317018838765051,
0.333333333333333,0.317018838765051,0.333333333333333,0.317018838765051,
0.333333333333333,0.317018838765051,0.333333333333333,0.317018838765051,
0.333333333333333,0.317018838765051,0.333333333333333,0.317018838765051,
0.333333333333333,0.317018838765051,0.333333333333333,0.317018838765051,
0.333333333333333,0.317018838765051,0.333333333333333,0.317018838765051,
0.333333333333333,0.317018838765051,0.333333333333333,0.317018838765051,
0.333333333333333,0.317018838765051,0.333333333333333,0.317018838765051,
0.333333333333333,0.317018838765051,0.333333333333333,0.317018838765051,
0.333333333333333,0.317018838765051,0.333333333333333,0.317018838765051,
0.333333333333333,0.317018838765051,0.333333333333333,0.317018838765051,
0.333333333333333,0.317018838765051,0.333333333333333,0.317018838765051,
0.333333333333333,0.317018838765051,0.333333333333333,0.317018838765051,
0.333333333333333,0.317018838765051,0.333333333333333,0.317018838765051,
0.333333333333333,0.317018838765051,0.333333333333333,0.317018838765051,
0.333333333333333,0.317018838765051,0.333333333333333,0.317018838765051,
0.333333333333333,0.317018838765051,0.333333333333333,0.317018838765051,
0.333333333333333,0.317018838765051,0.333333333333333,0.317018838765051,
0.333333333333333,0.317018838765051,0.333333333333333,0.317018838765051,
0.333333333333333,0.317018838765051,0.333333333333333,0.317018838765051,
0.333333333333333,0.317018838765051,0.333333333333333,0.317018838765051,
0.333333333333333,0.317018838765051,0.333333333333333,0.317018838765051,
0.333333333333333,0.317018838765051,0.333333333333333,0.317018838765051,
0.333333333333333,0.317018838765051,0.333333333333333,0.317018838765051,
0.333333333333333,0.317018838765051,0.333333333333333,0.317018838765051,
0.333333333333333,0.317018838765051,0.333333333333333,0.317018838765051,
0.333333333333333,0.317018838765051,0.333333333333333,0.317018838765051,
0.333333333333333,0.317018838765051,0.333333333333333,0.317018838765051,
0.333333333333333,0.317018838765051,0.333333333333333,0.317018838765051,
0.333333333333333,0.317018838765051,0.333333333333333,0.317018838765051,
0.333333333333333,0.317018838765051,0.333333333333333,0.317018838765051,
0.333333333333333,0.317018838765051,0.333333333333333,0.317018838765051,
0.333333333333333,0.317018838765051,0.333333333333333,0.317018838765051,
0.333333333333333,0.317018838765051,0.333333333333333,0.317018838765051,
0.333333333333333,0.317018838765051,0.333333333333333,0.317018838765051,
0.333333333333333,0.317018838765051,0.333333333333333,0.317018838765051,
0.333333333333333,0.317018838765051,0.333333333333333,0.317018838765051,
0.333333333333333,0.317018838765051,0.333333333333333,0.317018838765051,
0.333333333333333,0.317018838765051,0.333333333333333,0.317018838765051,
0.333333333333333,0.317018838765051,0.333333333333333,0.317018838765051,
0.333333333333333,0.317018838765051,0.333333333333333,0.317018838765051,
0.333333333333333,0.317018838765051,0.333333333333333,0.317018838765051,
0.333333333333333,0.317018838765051,0.333333333333333,0.317018838765051,
0.333333333333333,0.317018838765051,0.333333333333333,0.317018838765051,
0.333333333333333,0.317018838765051,0.333333333333333),(0.333333333333333,
0.317018838765051,0.333333333333333,0.317018838765051,0.333333333333333,
0.317018838765051,0.333333333333333,0.317018838765051,0.333333333333333,
0.317018838765051,0.333333333333333,0.317018838765051,0.333333333333333,
0.317018838765051,0.333333333333333,0.317018838765051,0.333333333333333,
0.317018838765051,0.333333333333333,0.317018838765051,0.333333333333333,
0.317018838765051,0.333333333333333,0.317018838765051,0.333333333333333,
0.317018838765051,0.333333333333333,0.317018838765051,0.333333333333333,
0.317018838765051,0.333333333333333,0.317018838765051,0.333333333333333,
0.317018838765051,0.333333333333333,0.317018838765051,0.333333333333333,
0.317018838765051,0.333333333333333,0.317018838765051,0.333333333333333,
0.317018838765051,0.333333333333333,0.317018838765051,0.333333333333333,
0.317018838765051,0.333333333333333,0.317018838765051,0.333333333333333,
0.317018838765051,0.333333333333333,0.317018838765051,0.333333333333333,
0.317018838765051,0.333333333333333,0.317018838765051,0.333333333333333,
0.317018838765051,0.333333333333333,0.317018838765051,0.333333333333333,
0.317018838765051,0.333333333333333,0.317018838765051,0.333333333333333,
0.317018838765051,0.333333333333333,0.317018838765051,0.333333333333333,
0.317018838765051,0.333333333333333,0.317018838765051,0.333333333333333,
0.317018838765051,0.333333333333333,0.317018838765051,0.333333333333333,
0.317018838765051,0.333333333333333,0.317018838765051,0.333333333333333,
0.317018838765051,0.333333333333333,0.317018838765051,0.333333333333333,
0.317018838765051,0.333333333333333,0.317018838765051,0.333333333333333,
0.317018838765051,0.333333333333333,0.317018838765051,0.333333333333333,
0.317018838765051,0.333333333333333,0.317018838765051,0.333333333333333,
0.317018838765051,0.333333333333333,0.317018838765051,0.333333333333333,
0.317018838765051,0.333333333333333,0.317018838765051,0.333333333333333,
0.317018838765051,0.333333333333333,0.317018838765051,0.333333333333333,
0.317018838765051,0.333333333333333,0.317018838765051,0.333333333333333,
0.317018838765051,0.333333333333333,0.317018838765051,0.333333333333333,
0.317018838765051,0.333333333333333,0.317018838765051,0.333333333333333,
0.317018838765051,0.333333333333333,0.317018838765051,0.333333333333333,
0.317018838765051,0.333333333333333,0.317018838765051,0.333333333333333,
0.317018838765051,0.333333333333333,0.317018838765051,0.333333333333333,
0.317018838765051,0.333333333333333,0.317018838765051,0.333333333333333,
0.317018838765051,0.333333333333333,0.317018838765051,0.333333333333333,
0.317018838765051,0.333333333333333,0.317018838765051,0.333333333333333,
0.317018838765051,0.333333333333333,0.317018838765051,0.333333333333333,
0.317018838765051,0.333333333333333,0.317018838765051,0.333333333333333,
0.317018838765051,0.333333333333333,0.317018838765051,0.333333333333333,
0.317018838765051,0.333333333333333,0.317018838765051,0.333333333333333,
0.317018838765051,0.333333333333333,0.317018838765051,0.333333333333333,
0.317018838765051,0.333333333333333,0.317018838765051,0.333333333333333,
0.317018838765051,0.333333333333333,0.317018838765051,0.333333333333333,
0.317018838765051,0.333333333333333,0.317018838765051,0.333333333333333,
0.317018838765051,0.333333333333333,0.317018838765051,0.333333333333333,
0.317018838765051,0.333333333333333,0.317018838765051,0.333333333333333,
0.317018838765051,0.333333333333333,0.317018838765051,0.333333333333333,
0.317018838765051,0.333333333333333,0.317018838765051,0.333333333333333,
0.317018838765051,0.333333333333333,0.317018838765051,0.333333333333333,
0.317018838765051,0.333333333333333,0.317018838765051,0.333333333333333),
(1.,0.951056516295154,1.,0.951056516295154,1.,0.951056516295154,1.,0.951056516295154,
1.,0.951056516295154,1.,0.951056516295154,1.,0.951056516295154,1.,0.951056516295154,
1.,0.951056516295154,1.,0.951056516295154,1.,0.951056516295154,1.,0.951056516295154,
1.,0.951056516295154,1.,0.951056516295154,1.,0.951056516295154,1.,0.951056516295154,
1.,0.951056516295154,1.,0.951056516295154,1.,0.951056516295154,1.,0.951056516295154,
1.,0.951056516295154,1.,0.951056516295154,1.,0.951056516295154,1.,0.951056516295154,
1.,0.951056516295154,1.,0.951056516295154,1.,0.951056516295154,1.,0.951056516295154,
1.,0.951056516295154,1.,0.951056516295154,1.,0.951056516295154,1.,0.951056516295154,
1.,0.951056516295154,1.,0.951056516295154,1.,0.951056516295154,1.,0.951056516295154,
1.,0.951056516295154,1.,0.951056516295154,1.,0.951056516295154,1.,0.951056516295154,
1.,0.951056516295154,1.,0.951056516295154,1.,0.951056516295154,1.,0.951056516295154,
1.,0.951056516295154,1.,0.951056516295154,1.,0.951056516295154,1.,0.951056516295154,
1.,0.951056516295154,1.,0.951056516295154,1.,0.951056516295154,1.,0.951056516295154,
1.,0.951056516295154,1.,0.951056516295154,1.,0.951056516295154,1.,0.951056516295154,
1.,0.951056516295154,1.,0.951056516295154,1.,0.951056516295154,1.,0.951056516295154,
1.,0.951056516295154,1.,0.951056516295154,1.,0.951056516295154,1.,0.951056516295154,
1.,0.951056516295154,1.,0.951056516295154,1.,0.951056516295154,1.,0.951056516295154,
1.,0.951056516295154,1.,0.951056516295154,1.,0.951056516295154,1.,0.951056516295154,
1.,0.951056516295154,1.,0.951056516295154,1.,0.951056516295154,1.,0.951056516295154,
1.,0.951056516295154,1.,0.951056516295154,1.,0.951056516295154,1.,0.951056516295154,
1.,0.951056516295154,1.,0.951056516295154,1.,0.951056516295154,1.,0.951056516295154,
1.,0.951056516295154,1.,0.951056516295154,1.,0.951056516295154,1.,0.951056516295154,
1.,0.951056516295154,1.,0.951056516295154,1.,0.951056516295154,1.,0.951056516295154,
1.,0.951056516295154,1.,0.951056516295154,1.,0.951056516295154,1.,0.951056516295154,
1.,0.951056516295154,1.,0.951056516295154,1.,0.951056516295154,1.,0.951056516295154,
1.),(0.333333333333333,0.317018838765051,0.333333333333333,0.317018838765051,
0.333333333333333,0.317018838765051,0.333333333333333,0.317018838765051,
0.333333333333333,0.317018838765051,0.333333333333333,0.317018838765051,
0.333333333333333,0.317018838765051,0.333333333333333,0.317018838765051,
0.333333333333333,0.317018838765051,0.333333333333333,0.317018838765051,
0.333333333333333,0.317018838765051,0.333333333333333,0.317018838765051,
0.333333333333333,0.317018838765051,0.333333333333333,0.317018838765051,
0.333333333333333,0.317018838765051,0.333333333333333,0.317018838765051,
0.333333333333333,0.317018838765051,0.333333333333333,0.317018838765051,
0.333333333333333,0.317018838765051,0.333333333333333,0.317018838765051,
0.333333333333333,0.317018838765051,0.333333333333333,0.317018838765051,
0.333333333333333,0.317018838765051,0.333333333333333,0.317018838765051,
0.333333333333333,0.317018838765051,0.333333333333333,0.317018838765051,
0.333333333333333,0.317018838765051,0.333333333333333,0.317018838765051,
0.333333333333333,0.317018838765051,0.333333333333333,0.317018838765051,
0.333333333333333,0.317018838765051,0.333333333333333,0.317018838765051,
0.333333333333333,0.317018838765051,0.333333333333333,0.317018838765051,
0.333333333333333,0.317018838765051,0.333333333333333,0.317018838765051,
0.333333333333333,0.317018838765051,0.333333333333333,0.317018838765051,
0.333333333333333,0.317018838765051,0.333333333333333,0.317018838765051,
0.333333333333333,0.317018838765051,0.333333333333333,0.317018838765051,
0.333333333333333,0.317018838765051,0.333333333333333,0.317018838765051,
0.333333333333333,0.317018838765051,0.333333333333333,0.317018838765051,
0.333333333333333,0.317018838765051,0.333333333333333,0.317018838765051,
0.333333333333333,0.317018838765051,0.333333333333333,0.317018838765051,
0.333333333333333,0.317018838765051,0.333333333333333,0.317018838765051,
0.333333333333333,0.317018838765051,0.333333333333333,0.317018838765051,
0.333333333333333,0.317018838765051,0.333333333333333,0.317018838765051,
0.333333333333333,0.317018838765051,0.333333333333333,0.317018838765051,
0.333333333333333,0.317018838765051,0.333333333333333,0.317018838765051,
0.333333333333333,0.317018838765051,0.333333333333333,0.317018838765051,
0.333333333333333,0.317018838765051,0.333333333333333,0.317018838765051,
0.333333333333333,0.317018838765051,0.333333333333333,0.317018838765051,
0.333333333333333,0.317018838765051,0.333333333333333,0.317018838765051,
0.333333333333333,0.317018838765051,0.333333333333333,0.317018838765051,
0.333333333333333,0.317018838765051,0.333333333333333,0.317018838765051,
0.333333333333333,0.317018838765051,0.333333333333333,0.317018838765051,
0.333333333333333,0.317018838765051,0.333333333333333,0.317018838765051,
0.333333333333333,0.317018838765051,0.333333333333333,0.317018838765051,
0.333333333333333,0.317018838765051,0.333333333333333,0.317018838765051,
0.333333333333333,0.317018838765051,0.333333333333333,0.317018838765051,
0.333333333333333,0.317018838765051,0.333333333333333,0.317018838765051,
0.333333333333333,0.317018838765051,0.333333333333333,0.317018838765051,
0.333333333333333,0.317018838765051,0.333333333333333,0.317018838765051,
0.333333333333333,0.317018838765051,0.333333333333333,0.317018838765051,
0.333333333333333,0.317018838765051,0.333333333333333,0.317018838765051,
0.333333333333333,0.317018838765051,0.333333333333333,0.317018838765051,
0.333333333333333,0.317018838765051,0.333333333333333,0.317018838765051,
0.333333333333333,0.317018838765051,0.333333333333333,0.317018838765051,
0.333333333333333,0.317018838765051,0.333333333333333,0.317018838765051,
0.333333333333333),(0.333333333333333,0.317018838765051,0.333333333333333,
0.317018838765051,0.333333333333333,0.317018838765051,0.333333333333333,
0.317018838765051,0.333333333333333,0.317018838765051,0.333333333333333,
0.317018838765051,0.333333333333333,0.317018838765051,0.333333333333333,
0.317018838765051,0.333333333333333,0.317018838765051,0.333333333333333,
0.317018838765051,0.333333333333333,0.317018838765051,0.333333333333333,
0.317018838765051,0.333333333333333,0.317018838765051,0.333333333333333,
0.317018838765051,0.333333333333333,0.317018838765051,0.333333333333333,
0.317018838765051,0.333333333333333,0.317018838765051,0.333333333333333,
0.317018838765051,0.333333333333333,0.317018838765051,0.333333333333333,
0.317018838765051,0.333333333333333,0.317018838765051,0.333333333333333,
0.317018838765051,0.333333333333333,0.317018838765051,0.333333333333333,
0.317018838765051,0.333333333333333,0.317018838765051,0.333333333333333,
0.317018838765051,0.333333333333333,0.317018838765051,0.333333333333333,
0.317018838765051,0.333333333333333,0.317018838765051,0.333333333333333,
0.317018838765051,0.333333333333333,0.317018838765051,0.333333333333333,
0.317018838765051,0.333333333333333,0.317018838765051,0.333333333333333,
0.317018838765051,0.333333333333333,0.317018838765051,0.333333333333333,
0.317018838765051,0.333333333333333,0.317018838765051,0.333333333333333,
0.317018838765051,0.333333333333333,0.317018838765051,0.333333333333333,
0.317018838765051,0.333333333333333,0.317018838765051,0.333333333333333,
0.317018838765051,0.333333333333333,0.317018838765051,0.333333333333333,
0.317018838765051,0.333333333333333,0.317018838765051,0.333333333333333,
0.317018838765051,0.333333333333333,0.317018838765051,0.333333333333333,
0.317018838765051,0.333333333333333,0.317018838765051,0.333333333333333,
0.317018838765051,0.333333333333333,0.317018838765051,0.333333333333333,
0.317018838765051,0.333333333333333,0.317018838765051,0.333333333333333,
0.317018838765051,0.333333333333333,0.317018838765051,0.333333333333333,
0.317018838765051,0.333333333333333,0.317018838765051,0.333333333333333,
0.317018838765051,0.333333333333333,0.317018838765051,0.333333333333333,
0.317018838765051,0.333333333333333,0.317018838765051,0.333333333333333,
0.317018838765051,0.333333333333333,0.317018838765051,0.333333333333333,
0.317018838765051,0.333333333333333,0.317018838765051,0.333333333333333,
0.317018838765051,0.333333333333333,0.317018838765051,0.333333333333333,
0.317018838765051,0.333333333333333,0.317018838765051,0.333333333333333,
0.317018838765051,0.333333333333333,0.317018838765051,0.333333333333333,
0.317018838765051,0.333333333333333,0.317018838765051,0.333333333333333,
0.317018838765051,0.333333333333333,0.317018838765051,0.333333333333333,
0.317018838765051,0.333333333333333,0.317018838765051,0.333333333333333,
0.317018838765051,0.333333333333333,0.317018838765051,0.333333333333333,
0.317018838765051,0.333333333333333,0.317018838765051,0.333333333333333,
0.317018838765051,0.333333333333333,0.317018838765051,0.333333333333333,
0.317018838765051,0.333333333333333,0.317018838765051,0.333333333333333,
0.317018838765051,0.333333333333333,0.317018838765051,0.333333333333333,
0.317018838765051,0.333333333333333,0.317018838765051,0.333333333333333,
0.317018838765051,0.333333333333333,0.317018838765051,0.333333333333333,
0.317018838765051,0.333333333333333,0.317018838765051,0.333333333333333,
0.317018838765051,0.333333333333333,0.317018838765051,0.333333333333333,
0.317018838765051,0.333333333333333,0.317018838765051,0.333333333333333,
0.317018838765051,0.333333333333333,0.317018838765051,0.333333333333333,
0.317018838765051,0.333333333333333),(1.,0.951056516295154,1.,0.951056516295154,
1.,0.951056516295154,1.,0.951056516295154,1.,0.951056516295154,1.,0.951056516295154,
1.,0.951056516295154,1.,0.951056516295154,1.,0.951056516295154,1.,0.951056516295154,
1.,0.951056516295154,1.,0.951056516295154,1.,0.951056516295154,1.,0.951056516295154,
1.,0.951056516295154,1.,0.951056516295154,1.,0.951056516295154,1.,0.951056516295154,
1.,0.951056516295154,1.,0.951056516295154,1.,0.951056516295154,1.,0.951056516295154,
1.,0.951056516295154,1.,0.951056516295154,1.,0.951056516295154,1.,0.951056516295154,
1.,0.951056516295154,1.,0.951056516295154,1.,0.951056516295154,1.,0.951056516295154,
1.,0.951056516295154,1.,0.951056516295154,1.,0.951056516295154,1.,0.951056516295154,
1.,0.951056516295154,1.,0.951056516295154,1.,0.951056516295154,1.,0.951056516295154,
1.,0.951056516295154,1.,0.951056516295154,1.,0.951056516295154,1.,0.951056516295154,
1.,0.951056516295154,1.,0.951056516295154,1.,0.951056516295154,1.,0.951056516295154,
1.,0.951056516295154,1.,0.951056516295154,1.,0.951056516295154,1.,0.951056516295154,
1.,0.951056516295154,1.,0.951056516295154,1.,0.951056516295154,1.,0.951056516295154,
1.,0.951056516295154,1.,0.951056516295154,1.,0.951056516295154,1.,0.951056516295154,
1.,0.951056516295154,1.,0.951056516295154,1.,0.951056516295154,1.,0.951056516295154,
1.,0.951056516295154,1.,0.951056516295154,1.,0.951056516295154,1.,0.951056516295154,
1.,0.951056516295154,1.,0.951056516295154,1.,0.951056516295154,1.,0.951056516295154,
1.,0.951056516295154,1.,0.951056516295154,1.,0.951056516295154,1.,0.951056516295154,
1.,0.951056516295154,1.,0.951056516295154,1.,0.951056516295154,1.,0.951056516295154,
1.,0.951056516295154,1.,0.951056516295154,1.,0.951056516295154,1.,0.951056516295154,
1.,0.951056516295154,1.,0.951056516295154,1.,0.951056516295154,1.,0.951056516295154,
1.,0.951056516295154,1.,0.951056516295154,1.,0.951056516295154,1.,0.951056516295154,
1.,0.951056516295154,1.,0.951056516295154,1.,0.951056516295154,1.,0.951056516295154,
1.,0.951056516295154,1.,0.951056516295154,1.,0.951056516295154,1.,0.951056516295154,
1.,0.951056516295154,1.,0.951056516295154,1.)))
REPRESENTATION_ITEM('')
SURFACE()
);
#96=(
BOUNDED_SURFACE()
B_SPLINE_SURFACE(3,2,((#5662,#5663,#5664,#5665,#5666,#5667,#5668,#5669,
#5670,#5671,#5672,#5673,#5674,#5675,#5676,#5677,#5678,#5679,#5680,#5681,
#5682,#5683,#5684,#5685,#5686,#5687,#5688,#5689,#5690,#5691,#5692,#5693,
#5694,#5695,#5696,#5697,#5698,#5699,#5700,#5701,#5702,#5703,#5704,#5705,
#5706,#5707,#5708,#5709,#5710,#5711,#5712,#5713,#5714,#5715,#5716,#5717,
#5718,#5719,#5720,#5721,#5722,#5723,#5724,#5725,#5726,#5727,#5728,#5729,
#5730,#5731,#5732,#5733,#5734,#5735,#5736,#5737,#5738,#5739,#5740,#5741,
#5742,#5743,#5744,#5745,#5746,#5747,#5748,#5749,#5750,#5751,#5752,#5753,
#5754,#5755,#5756,#5757,#5758,#5759,#5760,#5761,#5762,#5763,#5764,#5765,
#5766,#5767,#5768,#5769,#5770,#5771,#5772,#5773,#5774,#5775,#5776,#5777,
#5778,#5779,#5780,#5781,#5782,#5783,#5784,#5785,#5786,#5787,#5788,#5789,
#5790,#5791,#5792,#5793,#5794,#5795,#5796,#5797,#5798,#5799,#5800,#5801,
#5802,#5803,#5804,#5805,#5806,#5807,#5808,#5809,#5810,#5811,#5812,#5813,
#5814,#5815,#5816,#5817,#5818,#5819,#5820,#5821,#5822,#5823,#5824,#5825,
#5826,#5827,#5828,#5829,#5830,#5831,#5832,#5833,#5834,#5835,#5836,#5837,
#5838,#5839,#5840,#5841,#5842,#5843,#5844,#5845,#5846,#5847,#5848,#5849,
#5850,#5851,#5852,#5853,#5854,#5855,#5856,#5857,#5858,#5859,#5860,#5861,
#5862),(#5863,#5864,#5865,#5866,#5867,#5868,#5869,#5870,#5871,#5872,#5873,
#5874,#5875,#5876,#5877,#5878,#5879,#5880,#5881,#5882,#5883,#5884,#5885,
#5886,#5887,#5888,#5889,#5890,#5891,#5892,#5893,#5894,#5895,#5896,#5897,
#5898,#5899,#5900,#5901,#5902,#5903,#5904,#5905,#5906,#5907,#5908,#5909,
#5910,#5911,#5912,#5913,#5914,#5915,#5916,#5917,#5918,#5919,#5920,#5921,
#5922,#5923,#5924,#5925,#5926,#5927,#5928,#5929,#5930,#5931,#5932,#5933,
#5934,#5935,#5936,#5937,#5938,#5939,#5940,#5941,#5942,#5943,#5944,#5945,
#5946,#5947,#5948,#5949,#5950,#5951,#5952,#5953,#5954,#5955,#5956,#5957,
#5958,#5959,#5960,#5961,#5962,#5963,#5964,#5965,#5966,#5967,#5968,#5969,
#5970,#5971,#5972,#5973,#5974,#5975,#5976,#5977,#5978,#5979,#5980,#5981,
#5982,#5983,#5984,#5985,#5986,#5987,#5988,#5989,#5990,#5991,#5992,#5993,
#5994,#5995,#5996,#5997,#5998,#5999,#6000,#6001,#6002,#6003,#6004,#6005,
#6006,#6007,#6008,#6009,#6010,#6011,#6012,#6013,#6014,#6015,#6016,#6017,
#6018,#6019,#6020,#6021,#6022,#6023,#6024,#6025,#6026,#6027,#6028,#6029,
#6030,#6031,#6032,#6033,#6034,#6035,#6036,#6037,#6038,#6039,#6040,#6041,
#6042,#6043,#6044,#6045,#6046,#6047,#6048,#6049,#6050,#6051,#6052,#6053,
#6054,#6055,#6056,#6057,#6058,#6059,#6060,#6061,#6062,#6063),(#6064,#6065,
#6066,#6067,#6068,#6069,#6070,#6071,#6072,#6073,#6074,#6075,#6076,#6077,
#6078,#6079,#6080,#6081,#6082,#6083,#6084,#6085,#6086,#6087,#6088,#6089,
#6090,#6091,#6092,#6093,#6094,#6095,#6096,#6097,#6098,#6099,#6100,#6101,
#6102,#6103,#6104,#6105,#6106,#6107,#6108,#6109,#6110,#6111,#6112,#6113,
#6114,#6115,#6116,#6117,#6118,#6119,#6120,#6121,#6122,#6123,#6124,#6125,
#6126,#6127,#6128,#6129,#6130,#6131,#6132,#6133,#6134,#6135,#6136,#6137,
#6138,#6139,#6140,#6141,#6142,#6143,#6144,#6145,#6146,#6147,#6148,#6149,
#6150,#6151,#6152,#6153,#6154,#6155,#6156,#6157,#6158,#6159,#6160,#6161,
#6162,#6163,#6164,#6165,#6166,#6167,#6168,#6169,#6170,#6171,#6172,#6173,
#6174,#6175,#6176,#6177,#6178,#6179,#6180,#6181,#6182,#6183,#6184,#6185,
#6186,#6187,#6188,#6189,#6190,#6191,#6192,#6193,#6194,#6195,#6196,#6197,
#6198,#6199,#6200,#6201,#6202,#6203,#6204,#6205,#6206,#6207,#6208,#6209,
#6210,#6211,#6212,#6213,#6214,#6215,#6216,#6217,#6218,#6219,#6220,#6221,
#6222,#6223,#6224,#6225,#6226,#6227,#6228,#6229,#6230,#6231,#6232,#6233,
#6234,#6235,#6236,#6237,#6238,#6239,#6240,#6241,#6242,#6243,#6244,#6245,
#6246,#6247,#6248,#6249,#6250,#6251,#6252,#6253,#6254,#6255,#6256,#6257,
#6258,#6259,#6260,#6261,#6262,#6263,#6264),(#6265,#6266,#6267,#6268,#6269,
#6270,#6271,#6272,#6273,#6274,#6275,#6276,#6277,#6278,#6279,#6280,#6281,
#6282,#6283,#6284,#6285,#6286,#6287,#6288,#6289,#6290,#6291,#6292,#6293,
#6294,#6295,#6296,#6297,#6298,#6299,#6300,#6301,#6302,#6303,#6304,#6305,
#6306,#6307,#6308,#6309,#6310,#6311,#6312,#6313,#6314,#6315,#6316,#6317,
#6318,#6319,#6320,#6321,#6322,#6323,#6324,#6325,#6326,#6327,#6328,#6329,
#6330,#6331,#6332,#6333,#6334,#6335,#6336,#6337,#6338,#6339,#6340,#6341,
#6342,#6343,#6344,#6345,#6346,#6347,#6348,#6349,#6350,#6351,#6352,#6353,
#6354,#6355,#6356,#6357,#6358,#6359,#6360,#6361,#6362,#6363,#6364,#6365,
#6366,#6367,#6368,#6369,#6370,#6371,#6372,#6373,#6374,#6375,#6376,#6377,
#6378,#6379,#6380,#6381,#6382,#6383,#6384,#6385,#6386,#6387,#6388,#6389,
#6390,#6391,#6392,#6393,#6394,#6395,#6396,#6397,#6398,#6399,#6400,#6401,
#6402,#6403,#6404,#6405,#6406,#6407,#6408,#6409,#6410,#6411,#6412,#6413,
#6414,#6415,#6416,#6417,#6418,#6419,#6420,#6421,#6422,#6423,#6424,#6425,
#6426,#6427,#6428,#6429,#6430,#6431,#6432,#6433,#6434,#6435,#6436,#6437,
#6438,#6439,#6440,#6441,#6442,#6443,#6444,#6445,#6446,#6447,#6448,#6449,
#6450,#6451,#6452,#6453,#6454,#6455,#6456,#6457,#6458,#6459,#6460,#6461,
#6462,#6463,#6464,#6465),(#6466,#6467,#6468,#6469,#6470,#6471,#6472,#6473,
#6474,#6475,#6476,#6477,#6478,#6479,#6480,#6481,#6482,#6483,#6484,#6485,
#6486,#6487,#6488,#6489,#6490,#6491,#6492,#6493,#6494,#6495,#6496,#6497,
#6498,#6499,#6500,#6501,#6502,#6503,#6504,#6505,#6506,#6507,#6508,#6509,
#6510,#6511,#6512,#6513,#6514,#6515,#6516,#6517,#6518,#6519,#6520,#6521,
#6522,#6523,#6524,#6525,#6526,#6527,#6528,#6529,#6530,#6531,#6532,#6533,
#6534,#6535,#6536,#6537,#6538,#6539,#6540,#6541,#6542,#6543,#6544,#6545,
#6546,#6547,#6548,#6549,#6550,#6551,#6552,#6553,#6554,#6555,#6556,#6557,
#6558,#6559,#6560,#6561,#6562,#6563,#6564,#6565,#6566,#6567,#6568,#6569,
#6570,#6571,#6572,#6573,#6574,#6575,#6576,#6577,#6578,#6579,#6580,#6581,
#6582,#6583,#6584,#6585,#6586,#6587,#6588,#6589,#6590,#6591,#6592,#6593,
#6594,#6595,#6596,#6597,#6598,#6599,#6600,#6601,#6602,#6603,#6604,#6605,
#6606,#6607,#6608,#6609,#6610,#6611,#6612,#6613,#6614,#6615,#6616,#6617,
#6618,#6619,#6620,#6621,#6622,#6623,#6624,#6625,#6626,#6627,#6628,#6629,
#6630,#6631,#6632,#6633,#6634,#6635,#6636,#6637,#6638,#6639,#6640,#6641,
#6642,#6643,#6644,#6645,#6646,#6647,#6648,#6649,#6650,#6651,#6652,#6653,
#6654,#6655,#6656,#6657,#6658,#6659,#6660,#6661,#6662,#6663,#6664,#6665,
#6666),(#6667,#6668,#6669,#6670,#6671,#6672,#6673,#6674,#6675,#6676,#6677,
#6678,#6679,#6680,#6681,#6682,#6683,#6684,#6685,#6686,#6687,#6688,#6689,
#6690,#6691,#6692,#6693,#6694,#6695,#6696,#6697,#6698,#6699,#6700,#6701,
#6702,#6703,#6704,#6705,#6706,#6707,#6708,#6709,#6710,#6711,#6712,#6713,
#6714,#6715,#6716,#6717,#6718,#6719,#6720,#6721,#6722,#6723,#6724,#6725,
#6726,#6727,#6728,#6729,#6730,#6731,#6732,#6733,#6734,#6735,#6736,#6737,
#6738,#6739,#6740,#6741,#6742,#6743,#6744,#6745,#6746,#6747,#6748,#6749,
#6750,#6751,#6752,#6753,#6754,#6755,#6756,#6757,#6758,#6759,#6760,#6761,
#6762,#6763,#6764,#6765,#6766,#6767,#6768,#6769,#6770,#6771,#6772,#6773,
#6774,#6775,#6776,#6777,#6778,#6779,#6780,#6781,#6782,#6783,#6784,#6785,
#6786,#6787,#6788,#6789,#6790,#6791,#6792,#6793,#6794,#6795,#6796,#6797,
#6798,#6799,#6800,#6801,#6802,#6803,#6804,#6805,#6806,#6807,#6808,#6809,
#6810,#6811,#6812,#6813,#6814,#6815,#6816,#6817,#6818,#6819,#6820,#6821,
#6822,#6823,#6824,#6825,#6826,#6827,#6828,#6829,#6830,#6831,#6832,#6833,
#6834,#6835,#6836,#6837,#6838,#6839,#6840,#6841,#6842,#6843,#6844,#6845,
#6846,#6847,#6848,#6849,#6850,#6851,#6852,#6853,#6854,#6855,#6856,#6857,
#6858,#6859,#6860,#6861,#6862,#6863,#6864,#6865,#6866,#6867),(#6868,#6869,
#6870,#6871,#6872,#6873,#6874,#6875,#6876,#6877,#6878,#6879,#6880,#6881,
#6882,#6883,#6884,#6885,#6886,#6887,#6888,#6889,#6890,#6891,#6892,#6893,
#6894,#6895,#6896,#6897,#6898,#6899,#6900,#6901,#6902,#6903,#6904,#6905,
#6906,#6907,#6908,#6909,#6910,#6911,#6912,#6913,#6914,#6915,#6916,#6917,
#6918,#6919,#6920,#6921,#6922,#6923,#6924,#6925,#6926,#6927,#6928,#6929,
#6930,#6931,#6932,#6933,#6934,#6935,#6936,#6937,#6938,#6939,#6940,#6941,
#6942,#6943,#6944,#6945,#6946,#6947,#6948,#6949,#6950,#6951,#6952,#6953,
#6954,#6955,#6956,#6957,#6958,#6959,#6960,#6961,#6962,#6963,#6964,#6965,
#6966,#6967,#6968,#6969,#6970,#6971,#6972,#6973,#6974,#6975,#6976,#6977,
#6978,#6979,#6980,#6981,#6982,#6983,#6984,#6985,#6986,#6987,#6988,#6989,
#6990,#6991,#6992,#6993,#6994,#6995,#6996,#6997,#6998,#6999,#7000,#7001,
#7002,#7003,#7004,#7005,#7006,#7007,#7008,#7009,#7010,#7011,#7012,#7013,
#7014,#7015,#7016,#7017,#7018,#7019,#7020,#7021,#7022,#7023,#7024,#7025,
#7026,#7027,#7028,#7029,#7030,#7031,#7032,#7033,#7034,#7035,#7036,#7037,
#7038,#7039,#7040,#7041,#7042,#7043,#7044,#7045,#7046,#7047,#7048,#7049,
#7050,#7051,#7052,#7053,#7054,#7055,#7056,#7057,#7058,#7059,#7060,#7061,
#7062,#7063,#7064,#7065,#7066,#7067,#7068)),.UNSPECIFIED.,.T.,.F.,.F.)
B_SPLINE_SURFACE_WITH_KNOTS((4,3,4),(3,2,2,2,2,2,2,2,2,2,2,2,2,2,2,2,2,
2,2,2,2,2,2,2,2,2,2,2,2,2,2,2,2,2,2,2,2,2,2,2,2,2,2,2,2,2,2,2,2,2,2,2,2,
2,2,2,2,2,2,2,2,2,2,2,2,2,2,2,2,2,2,2,2,2,2,2,2,2,2,2,2,2,2,2,2,2,2,2,2,
2,2,2,2,2,2,2,2,2,2,2,3),(0.,0.5,1.),(0.,0.01,0.02,0.03,0.04,0.05,0.06,
0.07,0.08,0.09,0.1,0.11,0.12,0.13,0.14,0.15,0.16,0.17,0.18,0.19,0.2,0.21,
0.22,0.23,0.24,0.25,0.26,0.27,0.28,0.29,0.3,0.31,0.32,0.33,0.34,0.35,0.36,
0.37,0.38,0.39,0.4,0.41,0.42,0.43,0.44,0.45,0.46,0.47,0.48,0.49,0.5,0.51,
0.52,0.53,0.54,0.55,0.56,0.57,0.58,0.59,0.6,0.61,0.62,0.63,0.64,0.65,0.66,
0.67,0.68,0.69,0.7,0.71,0.72,0.73,0.74,0.75,0.76,0.77,0.78,0.79,0.8,0.81,
0.82,0.83,0.84,0.85,0.86,0.87,0.88,0.89,0.9,0.91,0.92,0.93,0.94,0.95,0.96,
0.97,0.98,0.99,1.),.UNSPECIFIED.)
GEOMETRIC_REPRESENTATION_ITEM()
RATIONAL_B_SPLINE_SURFACE(((1.,0.951056516295154,1.,0.951056516295154,1.,
0.951056516295154,1.,0.951056516295154,1.,0.951056516295154,1.,0.951056516295154,
1.,0.951056516295154,1.,0.951056516295154,1.,0.951056516295154,1.,0.951056516295154,
1.,0.951056516295154,1.,0.951056516295154,1.,0.951056516295154,1.,0.951056516295154,
1.,0.951056516295154,1.,0.951056516295154,1.,0.951056516295154,1.,0.951056516295154,
1.,0.951056516295154,1.,0.951056516295154,1.,0.951056516295154,1.,0.951056516295154,
1.,0.951056516295154,1.,0.951056516295154,1.,0.951056516295154,1.,0.951056516295154,
1.,0.951056516295154,1.,0.951056516295154,1.,0.951056516295154,1.,0.951056516295154,
1.,0.951056516295154,1.,0.951056516295154,1.,0.951056516295154,1.,0.951056516295154,
1.,0.951056516295154,1.,0.951056516295154,1.,0.951056516295154,1.,0.951056516295154,
1.,0.951056516295154,1.,0.951056516295154,1.,0.951056516295154,1.,0.951056516295154,
1.,0.951056516295154,1.,0.951056516295154,1.,0.951056516295154,1.,0.951056516295154,
1.,0.951056516295154,1.,0.951056516295154,1.,0.951056516295154,1.,0.951056516295154,
1.,0.951056516295154,1.,0.951056516295154,1.,0.951056516295154,1.,0.951056516295154,
1.,0.951056516295154,1.,0.951056516295154,1.,0.951056516295154,1.,0.951056516295154,
1.,0.951056516295154,1.,0.951056516295154,1.,0.951056516295154,1.,0.951056516295154,
1.,0.951056516295154,1.,0.951056516295154,1.,0.951056516295154,1.,0.951056516295154,
1.,0.951056516295154,1.,0.951056516295154,1.,0.951056516295154,1.,0.951056516295154,
1.,0.951056516295154,1.,0.951056516295154,1.,0.951056516295154,1.,0.951056516295154,
1.,0.951056516295154,1.,0.951056516295154,1.,0.951056516295154,1.,0.951056516295154,
1.,0.951056516295154,1.,0.951056516295154,1.,0.951056516295154,1.,0.951056516295154,
1.,0.951056516295154,1.,0.951056516295154,1.,0.951056516295154,1.,0.951056516295154,
1.,0.951056516295154,1.,0.951056516295154,1.,0.951056516295154,1.,0.951056516295154,
1.,0.951056516295154,1.,0.951056516295154,1.,0.951056516295154,1.,0.951056516295154,
1.,0.951056516295154,1.,0.951056516295154,1.,0.951056516295154,1.,0.951056516295154,
1.,0.951056516295154,1.,0.951056516295154,1.),(0.333333333333333,0.317018838765051,
0.333333333333333,0.317018838765051,0.333333333333333,0.317018838765051,
0.333333333333333,0.317018838765051,0.333333333333333,0.317018838765051,
0.333333333333333,0.317018838765051,0.333333333333333,0.317018838765051,
0.333333333333333,0.317018838765051,0.333333333333333,0.317018838765051,
0.333333333333333,0.317018838765051,0.333333333333333,0.317018838765051,
0.333333333333333,0.317018838765051,0.333333333333333,0.317018838765051,
0.333333333333333,0.317018838765051,0.333333333333333,0.317018838765051,
0.333333333333333,0.317018838765051,0.333333333333333,0.317018838765051,
0.333333333333333,0.317018838765051,0.333333333333333,0.317018838765051,
0.333333333333333,0.317018838765051,0.333333333333333,0.317018838765051,
0.333333333333333,0.317018838765051,0.333333333333333,0.317018838765051,
0.333333333333333,0.317018838765051,0.333333333333333,0.317018838765051,
0.333333333333333,0.317018838765051,0.333333333333333,0.317018838765051,
0.333333333333333,0.317018838765051,0.333333333333333,0.317018838765051,
0.333333333333333,0.317018838765051,0.333333333333333,0.317018838765051,
0.333333333333333,0.317018838765051,0.333333333333333,0.317018838765051,
0.333333333333333,0.317018838765051,0.333333333333333,0.317018838765051,
0.333333333333333,0.317018838765051,0.333333333333333,0.317018838765051,
0.333333333333333,0.317018838765051,0.333333333333333,0.317018838765051,
0.333333333333333,0.317018838765051,0.333333333333333,0.317018838765051,
0.333333333333333,0.317018838765051,0.333333333333333,0.317018838765051,
0.333333333333333,0.317018838765051,0.333333333333333,0.317018838765051,
0.333333333333333,0.317018838765051,0.333333333333333,0.317018838765051,
0.333333333333333,0.317018838765051,0.333333333333333,0.317018838765051,
0.333333333333333,0.317018838765051,0.333333333333333,0.317018838765051,
0.333333333333333,0.317018838765051,0.333333333333333,0.317018838765051,
0.333333333333333,0.317018838765051,0.333333333333333,0.317018838765051,
0.333333333333333,0.317018838765051,0.333333333333333,0.317018838765051,
0.333333333333333,0.317018838765051,0.333333333333333,0.317018838765051,
0.333333333333333,0.317018838765051,0.333333333333333,0.317018838765051,
0.333333333333333,0.317018838765051,0.333333333333333,0.317018838765051,
0.333333333333333,0.317018838765051,0.333333333333333,0.317018838765051,
0.333333333333333,0.317018838765051,0.333333333333333,0.317018838765051,
0.333333333333333,0.317018838765051,0.333333333333333,0.317018838765051,
0.333333333333333,0.317018838765051,0.333333333333333,0.317018838765051,
0.333333333333333,0.317018838765051,0.333333333333333,0.317018838765051,
0.333333333333333,0.317018838765051,0.333333333333333,0.317018838765051,
0.333333333333333,0.317018838765051,0.333333333333333,0.317018838765051,
0.333333333333333,0.317018838765051,0.333333333333333,0.317018838765051,
0.333333333333333,0.317018838765051,0.333333333333333,0.317018838765051,
0.333333333333333,0.317018838765051,0.333333333333333,0.317018838765051,
0.333333333333333,0.317018838765051,0.333333333333333,0.317018838765051,
0.333333333333333,0.317018838765051,0.333333333333333,0.317018838765051,
0.333333333333333,0.317018838765051,0.333333333333333,0.317018838765051,
0.333333333333333,0.317018838765051,0.333333333333333,0.317018838765051,
0.333333333333333,0.317018838765051,0.333333333333333,0.317018838765051,
0.333333333333333,0.317018838765051,0.333333333333333,0.317018838765051,
0.333333333333333,0.317018838765051,0.333333333333333,0.317018838765051,
0.333333333333333,0.317018838765051,0.333333333333333,0.317018838765051,
0.333333333333333,0.317018838765051,0.333333333333333),(0.333333333333333,
0.317018838765051,0.333333333333333,0.317018838765051,0.333333333333333,
0.317018838765051,0.333333333333333,0.317018838765051,0.333333333333333,
0.317018838765051,0.333333333333333,0.317018838765051,0.333333333333333,
0.317018838765051,0.333333333333333,0.317018838765051,0.333333333333333,
0.317018838765051,0.333333333333333,0.317018838765051,0.333333333333333,
0.317018838765051,0.333333333333333,0.317018838765051,0.333333333333333,
0.317018838765051,0.333333333333333,0.317018838765051,0.333333333333333,
0.317018838765051,0.333333333333333,0.317018838765051,0.333333333333333,
0.317018838765051,0.333333333333333,0.317018838765051,0.333333333333333,
0.317018838765051,0.333333333333333,0.317018838765051,0.333333333333333,
0.317018838765051,0.333333333333333,0.317018838765051,0.333333333333333,
0.317018838765051,0.333333333333333,0.317018838765051,0.333333333333333,
0.317018838765051,0.333333333333333,0.317018838765051,0.333333333333333,
0.317018838765051,0.333333333333333,0.317018838765051,0.333333333333333,
0.317018838765051,0.333333333333333,0.317018838765051,0.333333333333333,
0.317018838765051,0.333333333333333,0.317018838765051,0.333333333333333,
0.317018838765051,0.333333333333333,0.317018838765051,0.333333333333333,
0.317018838765051,0.333333333333333,0.317018838765051,0.333333333333333,
0.317018838765051,0.333333333333333,0.317018838765051,0.333333333333333,
0.317018838765051,0.333333333333333,0.317018838765051,0.333333333333333,
0.317018838765051,0.333333333333333,0.317018838765051,0.333333333333333,
0.317018838765051,0.333333333333333,0.317018838765051,0.333333333333333,
0.317018838765051,0.333333333333333,0.317018838765051,0.333333333333333,
0.317018838765051,0.333333333333333,0.317018838765051,0.333333333333333,
0.317018838765051,0.333333333333333,0.317018838765051,0.333333333333333,
0.317018838765051,0.333333333333333,0.317018838765051,0.333333333333333,
0.317018838765051,0.333333333333333,0.317018838765051,0.333333333333333,
0.317018838765051,0.333333333333333,0.317018838765051,0.333333333333333,
0.317018838765051,0.333333333333333,0.317018838765051,0.333333333333333,
0.317018838765051,0.333333333333333,0.317018838765051,0.333333333333333,
0.317018838765051,0.333333333333333,0.317018838765051,0.333333333333333,
0.317018838765051,0.333333333333333,0.317018838765051,0.333333333333333,
0.317018838765051,0.333333333333333,0.317018838765051,0.333333333333333,
0.317018838765051,0.333333333333333,0.317018838765051,0.333333333333333,
0.317018838765051,0.333333333333333,0.317018838765051,0.333333333333333,
0.317018838765051,0.333333333333333,0.317018838765051,0.333333333333333,
0.317018838765051,0.333333333333333,0.317018838765051,0.333333333333333,
0.317018838765051,0.333333333333333,0.317018838765051,0.333333333333333,
0.317018838765051,0.333333333333333,0.317018838765051,0.333333333333333,
0.317018838765051,0.333333333333333,0.317018838765051,0.333333333333333,
0.317018838765051,0.333333333333333,0.317018838765051,0.333333333333333,
0.317018838765051,0.333333333333333,0.317018838765051,0.333333333333333,
0.317018838765051,0.333333333333333,0.317018838765051,0.333333333333333,
0.317018838765051,0.333333333333333,0.317018838765051,0.333333333333333,
0.317018838765051,0.333333333333333,0.317018838765051,0.333333333333333,
0.317018838765051,0.333333333333333,0.317018838765051,0.333333333333333,
0.317018838765051,0.333333333333333,0.317018838765051,0.333333333333333,
0.317018838765051,0.333333333333333,0.317018838765051,0.333333333333333,
0.317018838765051,0.333333333333333,0.317018838765051,0.333333333333333,
0.317018838765051,0.333333333333333,0.317018838765051,0.333333333333333),
(1.,0.951056516295154,1.,0.951056516295154,1.,0.951056516295154,1.,0.951056516295154,
1.,0.951056516295154,1.,0.951056516295154,1.,0.951056516295154,1.,0.951056516295154,
1.,0.951056516295154,1.,0.951056516295154,1.,0.951056516295154,1.,0.951056516295154,
1.,0.951056516295154,1.,0.951056516295154,1.,0.951056516295154,1.,0.951056516295154,
1.,0.951056516295154,1.,0.951056516295154,1.,0.951056516295154,1.,0.951056516295154,
1.,0.951056516295154,1.,0.951056516295154,1.,0.951056516295154,1.,0.951056516295154,
1.,0.951056516295154,1.,0.951056516295154,1.,0.951056516295154,1.,0.951056516295154,
1.,0.951056516295154,1.,0.951056516295154,1.,0.951056516295154,1.,0.951056516295154,
1.,0.951056516295154,1.,0.951056516295154,1.,0.951056516295154,1.,0.951056516295154,
1.,0.951056516295154,1.,0.951056516295154,1.,0.951056516295154,1.,0.951056516295154,
1.,0.951056516295154,1.,0.951056516295154,1.,0.951056516295154,1.,0.951056516295154,
1.,0.951056516295154,1.,0.951056516295154,1.,0.951056516295154,1.,0.951056516295154,
1.,0.951056516295154,1.,0.951056516295154,1.,0.951056516295154,1.,0.951056516295154,
1.,0.951056516295154,1.,0.951056516295154,1.,0.951056516295154,1.,0.951056516295154,
1.,0.951056516295154,1.,0.951056516295154,1.,0.951056516295154,1.,0.951056516295154,
1.,0.951056516295154,1.,0.951056516295154,1.,0.951056516295154,1.,0.951056516295154,
1.,0.951056516295154,1.,0.951056516295154,1.,0.951056516295154,1.,0.951056516295154,
1.,0.951056516295154,1.,0.951056516295154,1.,0.951056516295154,1.,0.951056516295154,
1.,0.951056516295154,1.,0.951056516295154,1.,0.951056516295154,1.,0.951056516295154,
1.,0.951056516295154,1.,0.951056516295154,1.,0.951056516295154,1.,0.951056516295154,
1.,0.951056516295154,1.,0.951056516295154,1.,0.951056516295154,1.,0.951056516295154,
1.,0.951056516295154,1.,0.951056516295154,1.,0.951056516295154,1.,0.951056516295154,
1.,0.951056516295154,1.,0.951056516295154,1.,0.951056516295154,1.,0.951056516295154,
1.,0.951056516295154,1.,0.951056516295154,1.,0.951056516295154,1.,0.951056516295154,
1.,0.951056516295154,1.,0.951056516295154,1.,0.951056516295154,1.,0.951056516295154,
1.),(0.333333333333333,0.317018838765051,0.333333333333333,0.317018838765051,
0.333333333333333,0.317018838765051,0.333333333333333,0.317018838765051,
0.333333333333333,0.317018838765051,0.333333333333333,0.317018838765051,
0.333333333333333,0.317018838765051,0.333333333333333,0.317018838765051,
0.333333333333333,0.317018838765051,0.333333333333333,0.317018838765051,
0.333333333333333,0.317018838765051,0.333333333333333,0.317018838765051,
0.333333333333333,0.317018838765051,0.333333333333333,0.317018838765051,
0.333333333333333,0.317018838765051,0.333333333333333,0.317018838765051,
0.333333333333333,0.317018838765051,0.333333333333333,0.317018838765051,
0.333333333333333,0.317018838765051,0.333333333333333,0.317018838765051,
0.333333333333333,0.317018838765051,0.333333333333333,0.317018838765051,
0.333333333333333,0.317018838765051,0.333333333333333,0.317018838765051,
0.333333333333333,0.317018838765051,0.333333333333333,0.317018838765051,
0.333333333333333,0.317018838765051,0.333333333333333,0.317018838765051,
0.333333333333333,0.317018838765051,0.333333333333333,0.317018838765051,
0.333333333333333,0.317018838765051,0.333333333333333,0.317018838765051,
0.333333333333333,0.317018838765051,0.333333333333333,0.317018838765051,
0.333333333333333,0.317018838765051,0.333333333333333,0.317018838765051,
0.333333333333333,0.317018838765051,0.333333333333333,0.317018838765051,
0.333333333333333,0.317018838765051,0.333333333333333,0.317018838765051,
0.333333333333333,0.317018838765051,0.333333333333333,0.317018838765051,
0.333333333333333,0.317018838765051,0.333333333333333,0.317018838765051,
0.333333333333333,0.317018838765051,0.333333333333333,0.317018838765051,
0.333333333333333,0.317018838765051,0.333333333333333,0.317018838765051,
0.333333333333333,0.317018838765051,0.333333333333333,0.317018838765051,
0.333333333333333,0.317018838765051,0.333333333333333,0.317018838765051,
0.333333333333333,0.317018838765051,0.333333333333333,0.317018838765051,
0.333333333333333,0.317018838765051,0.333333333333333,0.317018838765051,
0.333333333333333,0.317018838765051,0.333333333333333,0.317018838765051,
0.333333333333333,0.317018838765051,0.333333333333333,0.317018838765051,
0.333333333333333,0.317018838765051,0.333333333333333,0.317018838765051,
0.333333333333333,0.317018838765051,0.333333333333333,0.317018838765051,
0.333333333333333,0.317018838765051,0.333333333333333,0.317018838765051,
0.333333333333333,0.317018838765051,0.333333333333333,0.317018838765051,
0.333333333333333,0.317018838765051,0.333333333333333,0.317018838765051,
0.333333333333333,0.317018838765051,0.333333333333333,0.317018838765051,
0.333333333333333,0.317018838765051,0.333333333333333,0.317018838765051,
0.333333333333333,0.317018838765051,0.333333333333333,0.317018838765051,
0.333333333333333,0.317018838765051,0.333333333333333,0.317018838765051,
0.333333333333333,0.317018838765051,0.333333333333333,0.317018838765051,
0.333333333333333,0.317018838765051,0.333333333333333,0.317018838765051,
0.333333333333333,0.317018838765051,0.333333333333333,0.317018838765051,
0.333333333333333,0.317018838765051,0.333333333333333,0.317018838765051,
0.333333333333333,0.317018838765051,0.333333333333333,0.317018838765051,
0.333333333333333,0.317018838765051,0.333333333333333,0.317018838765051,
0.333333333333333,0.317018838765051,0.333333333333333,0.317018838765051,
0.333333333333333,0.317018838765051,0.333333333333333,0.317018838765051,
0.333333333333333,0.317018838765051,0.333333333333333,0.317018838765051,
0.333333333333333,0.317018838765051,0.333333333333333,0.317018838765051,
0.333333333333333,0.317018838765051,0.333333333333333,0.317018838765051,
0.333333333333333),(0.333333333333333,0.317018838765051,0.333333333333333,
0.317018838765051,0.333333333333333,0.317018838765051,0.333333333333333,
0.317018838765051,0.333333333333333,0.317018838765051,0.333333333333333,
0.317018838765051,0.333333333333333,0.317018838765051,0.333333333333333,
0.317018838765051,0.333333333333333,0.317018838765051,0.333333333333333,
0.317018838765051,0.333333333333333,0.317018838765051,0.333333333333333,
0.317018838765051,0.333333333333333,0.317018838765051,0.333333333333333,
0.317018838765051,0.333333333333333,0.317018838765051,0.333333333333333,
0.317018838765051,0.333333333333333,0.317018838765051,0.333333333333333,
0.317018838765051,0.333333333333333,0.317018838765051,0.333333333333333,
0.317018838765051,0.333333333333333,0.317018838765051,0.333333333333333,
0.317018838765051,0.333333333333333,0.317018838765051,0.333333333333333,
0.317018838765051,0.333333333333333,0.317018838765051,0.333333333333333,
0.317018838765051,0.333333333333333,0.317018838765051,0.333333333333333,
0.317018838765051,0.333333333333333,0.317018838765051,0.333333333333333,
0.317018838765051,0.333333333333333,0.317018838765051,0.333333333333333,
0.317018838765051,0.333333333333333,0.317018838765051,0.333333333333333,
0.317018838765051,0.333333333333333,0.317018838765051,0.333333333333333,
0.317018838765051,0.333333333333333,0.317018838765051,0.333333333333333,
0.317018838765051,0.333333333333333,0.317018838765051,0.333333333333333,
0.317018838765051,0.333333333333333,0.317018838765051,0.333333333333333,
0.317018838765051,0.333333333333333,0.317018838765051,0.333333333333333,
0.317018838765051,0.333333333333333,0.317018838765051,0.333333333333333,
0.317018838765051,0.333333333333333,0.317018838765051,0.333333333333333,
0.317018838765051,0.333333333333333,0.317018838765051,0.333333333333333,
0.317018838765051,0.333333333333333,0.317018838765051,0.333333333333333,
0.317018838765051,0.333333333333333,0.317018838765051,0.333333333333333,
0.317018838765051,0.333333333333333,0.317018838765051,0.333333333333333,
0.317018838765051,0.333333333333333,0.317018838765051,0.333333333333333,
0.317018838765051,0.333333333333333,0.317018838765051,0.333333333333333,
0.317018838765051,0.333333333333333,0.317018838765051,0.333333333333333,
0.317018838765051,0.333333333333333,0.317018838765051,0.333333333333333,
0.317018838765051,0.333333333333333,0.317018838765051,0.333333333333333,
0.317018838765051,0.333333333333333,0.317018838765051,0.333333333333333,
0.317018838765051,0.333333333333333,0.317018838765051,0.333333333333333,
0.317018838765051,0.333333333333333,0.317018838765051,0.333333333333333,
0.317018838765051,0.333333333333333,0.317018838765051,0.333333333333333,
0.317018838765051,0.333333333333333,0.317018838765051,0.333333333333333,
0.317018838765051,0.333333333333333,0.317018838765051,0.333333333333333,
0.317018838765051,0.333333333333333,0.317018838765051,0.333333333333333,
0.317018838765051,0.333333333333333,0.317018838765051,0.333333333333333,
0.317018838765051,0.333333333333333,0.317018838765051,0.333333333333333,
0.317018838765051,0.333333333333333,0.317018838765051,0.333333333333333,
0.317018838765051,0.333333333333333,0.317018838765051,0.333333333333333,
0.317018838765051,0.333333333333333,0.317018838765051,0.333333333333333,
0.317018838765051,0.333333333333333,0.317018838765051,0.333333333333333,
0.317018838765051,0.333333333333333,0.317018838765051,0.333333333333333,
0.317018838765051,0.333333333333333,0.317018838765051,0.333333333333333,
0.317018838765051,0.333333333333333,0.317018838765051,0.333333333333333,
0.317018838765051,0.333333333333333,0.317018838765051,0.333333333333333,
0.317018838765051,0.333333333333333),(1.,0.951056516295154,1.,0.951056516295154,
1.,0.951056516295154,1.,0.951056516295154,1.,0.951056516295154,1.,0.951056516295154,
1.,0.951056516295154,1.,0.951056516295154,1.,0.951056516295154,1.,0.951056516295154,
1.,0.951056516295154,1.,0.951056516295154,1.,0.951056516295154,1.,0.951056516295154,
1.,0.951056516295154,1.,0.951056516295154,1.,0.951056516295154,1.,0.951056516295154,
1.,0.951056516295154,1.,0.951056516295154,1.,0.951056516295154,1.,0.951056516295154,
1.,0.951056516295154,1.,0.951056516295154,1.,0.951056516295154,1.,0.951056516295154,
1.,0.951056516295154,1.,0.951056516295154,1.,0.951056516295154,1.,0.951056516295154,
1.,0.951056516295154,1.,0.951056516295154,1.,0.951056516295154,1.,0.951056516295154,
1.,0.951056516295154,1.,0.951056516295154,1.,0.951056516295154,1.,0.951056516295154,
1.,0.951056516295154,1.,0.951056516295154,1.,0.951056516295154,1.,0.951056516295154,
1.,0.951056516295154,1.,0.951056516295154,1.,0.951056516295154,1.,0.951056516295154,
1.,0.951056516295154,1.,0.951056516295154,1.,0.951056516295154,1.,0.951056516295154,
1.,0.951056516295154,1.,0.951056516295154,1.,0.951056516295154,1.,0.951056516295154,
1.,0.951056516295154,1.,0.951056516295154,1.,0.951056516295154,1.,0.951056516295154,
1.,0.951056516295154,1.,0.951056516295154,1.,0.951056516295154,1.,0.951056516295154,
1.,0.951056516295154,1.,0.951056516295154,1.,0.951056516295154,1.,0.951056516295154,
1.,0.951056516295154,1.,0.951056516295154,1.,0.951056516295154,1.,0.951056516295154,
1.,0.951056516295154,1.,0.951056516295154,1.,0.951056516295154,1.,0.951056516295154,
1.,0.951056516295154,1.,0.951056516295154,1.,0.951056516295154,1.,0.951056516295154,
1.,0.951056516295154,1.,0.951056516295154,1.,0.951056516295154,1.,0.951056516295154,
1.,0.951056516295154,1.,0.951056516295154,1.,0.951056516295154,1.,0.951056516295154,
1.,0.951056516295154,1.,0.951056516295154,1.,0.951056516295154,1.,0.951056516295154,
1.,0.951056516295154,1.,0.951056516295154,1.,0.951056516295154,1.,0.951056516295154,
1.,0.951056516295154,1.,0.951056516295154,1.,0.951056516295154,1.,0.951056516295154,
1.,0.951056516295154,1.,0.951056516295154,1.)))
REPRESENTATION_ITEM('')
SURFACE()
);
#97=SHAPE_REPRESENTATION_RELATIONSHIP('SRR','None',#7665,#106);
#98=SHAPE_REPRESENTATION_RELATIONSHIP('SRR','None',#7666,#107);
#99=SHAPE_REPRESENTATION_RELATIONSHIP('SRR','None',#7667,#108);
#100=SHAPE_REPRESENTATION_RELATIONSHIP('SRR','None',#7668,#109);
#101=SHAPE_REPRESENTATION_RELATIONSHIP('SRR','None',#7669,#110);
#102=SHAPE_REPRESENTATION_RELATIONSHIP('SRR','None',#7670,#111);
#103=SHAPE_REPRESENTATION_RELATIONSHIP('SRR','None',#7671,#112);
#104=SHAPE_REPRESENTATION_RELATIONSHIP('SRR','None',#7672,#113);
#105=SHAPE_REPRESENTATION_RELATIONSHIP('SRR','None',#7673,#114);
#106=ADVANCED_BREP_SHAPE_REPRESENTATION('',(#136),#7618);
#107=ADVANCED_BREP_SHAPE_REPRESENTATION('',(#137),#7619);
#108=ADVANCED_BREP_SHAPE_REPRESENTATION('',(#138),#7620);
#109=ADVANCED_BREP_SHAPE_REPRESENTATION('',(#139),#7621);
#110=ADVANCED_BREP_SHAPE_REPRESENTATION('',(#140),#7622);
#111=ADVANCED_BREP_SHAPE_REPRESENTATION('',(#141),#7623);
#112=ADVANCED_BREP_SHAPE_REPRESENTATION('',(#142,#143,#144,#145,#146,#147,
#148,#149,#150,#151,#152,#153,#154),#7624);
#113=ADVANCED_BREP_SHAPE_REPRESENTATION('',(#155),#7625);
#114=ADVANCED_BREP_SHAPE_REPRESENTATION('',(#156),#7626);
#115=STYLED_ITEM('',(#7719),#136);
#116=STYLED_ITEM('',(#7720),#137);
#117=STYLED_ITEM('',(#7721),#138);
#118=STYLED_ITEM('',(#7722),#139);
#119=STYLED_ITEM('',(#7720),#140);
#120=STYLED_ITEM('',(#7723),#141);
#121=STYLED_ITEM('',(#7723),#142);
#122=STYLED_ITEM('',(#7723),#143);
#123=STYLED_ITEM('',(#7723),#144);
#124=STYLED_ITEM('',(#7723),#145);
#125=STYLED_ITEM('',(#7723),#146);
#126=STYLED_ITEM('',(#7723),#147);
#127=STYLED_ITEM('',(#7723),#148);
#128=STYLED_ITEM('',(#7723),#149);
#129=STYLED_ITEM('',(#7723),#150);
#130=STYLED_ITEM('',(#7723),#151);
#131=STYLED_ITEM('',(#7723),#152);
#132=STYLED_ITEM('',(#7723),#153);
#133=STYLED_ITEM('',(#7723),#154);
#134=STYLED_ITEM('',(#7719),#155);
#135=STYLED_ITEM('',(#7721),#156);
#136=MANIFOLD_SOLID_BREP('Body1',#2413);
#137=MANIFOLD_SOLID_BREP('Body1',#2414);
#138=MANIFOLD_SOLID_BREP('Body1',#2415);
#139=MANIFOLD_SOLID_BREP('Body1',#2416);
#140=MANIFOLD_SOLID_BREP('Body1',#2417);
#141=MANIFOLD_SOLID_BREP('Body1',#2418);
#142=MANIFOLD_SOLID_BREP('Body1',#2419);
#143=MANIFOLD_SOLID_BREP('Body2',#2420);
#144=MANIFOLD_SOLID_BREP('Body3',#2421);
#145=MANIFOLD_SOLID_BREP('Body4',#2422);
#146=MANIFOLD_SOLID_BREP('Body5',#2423);
#147=MANIFOLD_SOLID_BREP('Body6',#2424);
#148=MANIFOLD_SOLID_BREP('Body7',#2425);
#149=MANIFOLD_SOLID_BREP('Body8',#2426);
#150=MANIFOLD_SOLID_BREP('Body9',#2427);
#151=MANIFOLD_SOLID_BREP('Body10',#2428);
#152=MANIFOLD_SOLID_BREP('Body11',#2429);
#153=MANIFOLD_SOLID_BREP('Body12',#2430);
#154=MANIFOLD_SOLID_BREP('Body13',#2431);
#155=MANIFOLD_SOLID_BREP('Body1',#2432);
#156=MANIFOLD_SOLID_BREP('Body1',#2433);
#157=FACE_BOUND('',#474,.T.);
#158=FACE_BOUND('',#476,.T.);
#159=FACE_BOUND('',#479,.T.);
#160=FACE_BOUND('',#480,.T.);
#161=FACE_BOUND('',#481,.T.);
#162=FACE_BOUND('',#482,.T.);
#163=FACE_BOUND('',#483,.T.);
#164=FACE_BOUND('',#494,.T.);
#165=FACE_BOUND('',#497,.T.);
#166=FACE_BOUND('',#499,.T.);
#167=FACE_BOUND('',#504,.T.);
#168=FACE_BOUND('',#518,.T.);
#169=FACE_BOUND('',#519,.T.);
#170=FACE_BOUND('',#520,.T.);
#171=FACE_BOUND('',#521,.T.);
#172=FACE_BOUND('',#522,.T.);
#173=FACE_BOUND('',#524,.T.);
#174=FACE_BOUND('',#525,.T.);
#175=FACE_BOUND('',#526,.T.);
#176=FACE_BOUND('',#527,.T.);
#177=FACE_BOUND('',#528,.T.);
#178=FACE_BOUND('',#536,.T.);
#179=FACE_BOUND('',#605,.T.);
#180=FACE_BOUND('',#606,.T.);
#181=FACE_BOUND('',#607,.T.);
#182=FACE_BOUND('',#608,.T.);
#183=FACE_BOUND('',#609,.T.);
#184=FACE_BOUND('',#620,.T.);
#185=FACE_BOUND('',#621,.T.);
#186=FACE_BOUND('',#624,.T.);
#187=FACE_BOUND('',#625,.T.);
#188=FACE_BOUND('',#632,.T.);
#189=FACE_BOUND('',#634,.T.);
#190=FACE_BOUND('',#636,.T.);
#191=PLANE('',#2563);
#192=PLANE('',#2564);
#193=PLANE('',#2565);
#194=PLANE('',#2566);
#195=PLANE('',#2567);
#196=PLANE('',#2568);
#197=PLANE('',#2569);
#198=PLANE('',#2570);
#199=PLANE('',#2571);
#200=PLANE('',#2585);
#201=PLANE('',#2586);
#202=PLANE('',#2587);
#203=PLANE('',#2588);
#204=PLANE('',#2589);
#205=PLANE('',#2597);
#206=PLANE('',#2598);
#207=PLANE('',#2599);
#208=PLANE('',#2603);
#209=PLANE('',#2605);
#210=PLANE('',#2607);
#211=PLANE('',#2624);
#212=PLANE('',#2625);
#213=PLANE('',#2626);
#214=PLANE('',#2627);
#215=PLANE('',#2628);
#216=PLANE('',#2629);
#217=PLANE('',#2637);
#218=PLANE('',#2641);
#219=PLANE('',#2642);
#220=PLANE('',#2643);
#221=PLANE('',#2644);
#222=PLANE('',#2801);
#223=PLANE('',#2802);
#224=PLANE('',#2803);
#225=PLANE('',#2804);
#226=PLANE('',#2805);
#227=PLANE('',#2806);
#228=PLANE('',#2807);
#229=PLANE('',#2808);
#230=PLANE('',#2809);
#231=PLANE('',#2810);
#232=PLANE('',#2811);
#233=PLANE('',#2812);
#234=PLANE('',#2813);
#235=PLANE('',#2814);
#236=PLANE('',#2815);
#237=PLANE('',#2837);
#238=PLANE('',#2838);
#239=PLANE('',#2839);
#240=PLANE('',#2840);
#241=PLANE('',#2841);
#242=PLANE('',#2842);
#243=PLANE('',#2843);
#244=PLANE('',#2844);
#245=PLANE('',#2845);
#246=PLANE('',#2846);
#247=PLANE('',#2847);
#248=PLANE('',#2848);
#249=PLANE('',#2849);
#250=PLANE('',#2850);
#251=PLANE('',#2851);
#252=ELLIPSE('',#2553,5.6568542494923,3.99999999999995);
#253=ELLIPSE('',#2554,5.65685424949242,4.00000000000003);
#254=ELLIPSE('',#2556,5.65685424949242,4.00000000000003);
#255=CYLINDRICAL_SURFACE('',#2538,2.);
#256=CYLINDRICAL_SURFACE('',#2542,2.);
#257=CYLINDRICAL_SURFACE('',#2546,2.);
#258=CYLINDRICAL_SURFACE('',#2550,2.);
#259=CYLINDRICAL_SURFACE('',#2552,4.);
#260=CYLINDRICAL_SURFACE('',#2557,4.);
#261=CYLINDRICAL_SURFACE('',#2560,4.);
#262=CYLINDRICAL_SURFACE('',#2573,5.);
#263=CYLINDRICAL_SURFACE('',#2576,6.);
#264=CYLINDRICAL_SURFACE('',#2579,2.5);
#265=CYLINDRICAL_SURFACE('',#2582,4.);
#266=CYLINDRICAL_SURFACE('',#2591,2.5);
#267=CYLINDRICAL_SURFACE('',#2594,4.);
#268=CYLINDRICAL_SURFACE('',#2609,2.15);
#269=CYLINDRICAL_SURFACE('',#2612,2.15);
#270=CYLINDRICAL_SURFACE('',#2615,2.15);
#271=CYLINDRICAL_SURFACE('',#2618,2.15);
#272=CYLINDRICAL_SURFACE('',#2621,7.);
#273=CYLINDRICAL_SURFACE('',#2631,6.5);
#274=CYLINDRICAL_SURFACE('',#2634,8.);
#275=CYLINDRICAL_SURFACE('',#2639,8.);
#276=CYLINDRICAL_SURFACE('',#2654,0.999999999999999);
#277=CYLINDRICAL_SURFACE('',#2655,0.999999999999999);
#278=CYLINDRICAL_SURFACE('',#2664,0.999999999999999);
#279=CYLINDRICAL_SURFACE('',#2665,0.999999999999999);
#280=CYLINDRICAL_SURFACE('',#2674,0.999999999999999);
#281=CYLINDRICAL_SURFACE('',#2675,0.999999999999999);
#282=CYLINDRICAL_SURFACE('',#2684,0.999999999999999);
#283=CYLINDRICAL_SURFACE('',#2685,0.999999999999999);
#284=CYLINDRICAL_SURFACE('',#2694,0.999999999999999);
#285=CYLINDRICAL_SURFACE('',#2695,0.999999999999999);
#286=CYLINDRICAL_SURFACE('',#2704,0.999999999999999);
#287=CYLINDRICAL_SURFACE('',#2705,0.999999999999999);
#288=CYLINDRICAL_SURFACE('',#2714,0.999999999999999);
#289=CYLINDRICAL_SURFACE('',#2715,0.999999999999999);
#290=CYLINDRICAL_SURFACE('',#2724,0.999999999999999);
#291=CYLINDRICAL_SURFACE('',#2725,0.999999999999999);
#292=CYLINDRICAL_SURFACE('',#2734,0.999999999999999);
#293=CYLINDRICAL_SURFACE('',#2735,0.999999999999999);
#294=CYLINDRICAL_SURFACE('',#2744,0.999999999999999);
#295=CYLINDRICAL_SURFACE('',#2745,0.999999999999999);
#296=CYLINDRICAL_SURFACE('',#2754,0.999999999999999);
#297=CYLINDRICAL_SURFACE('',#2755,0.999999999999999);
#298=CYLINDRICAL_SURFACE('',#2764,0.999999999999999);
#299=CYLINDRICAL_SURFACE('',#2765,0.999999999999999);
#300=CYLINDRICAL_SURFACE('',#2774,0.999999999999999);
#301=CYLINDRICAL_SURFACE('',#2775,0.999999999999999);
#302=CYLINDRICAL_SURFACE('',#2793,2.15);
#303=CYLINDRICAL_SURFACE('',#2795,2.15);
#304=CYLINDRICAL_SURFACE('',#2797,2.15);
#305=CYLINDRICAL_SURFACE('',#2799,2.15);
#306=CYLINDRICAL_SURFACE('',#2831,2.);
#307=CYLINDRICAL_SURFACE('',#2832,3.8);
#308=FACE_OUTER_BOUND('',#462,.T.);
#309=FACE_OUTER_BOUND('',#463,.T.);
#310=FACE_OUTER_BOUND('',#464,.T.);
#311=FACE_OUTER_BOUND('',#465,.T.);
#312=FACE_OUTER_BOUND('',#466,.T.);
#313=FACE_OUTER_BOUND('',#467,.T.);
#314=FACE_OUTER_BOUND('',#468,.T.);
#315=FACE_OUTER_BOUND('',#469,.T.);
#316=FACE_OUTER_BOUND('',#470,.T.);
#317=FACE_OUTER_BOUND('',#471,.T.);
#318=FACE_OUTER_BOUND('',#472,.T.);
#319=FACE_OUTER_BOUND('',#473,.T.);
#320=FACE_OUTER_BOUND('',#475,.T.);
#321=FACE_OUTER_BOUND('',#477,.T.);
#322=FACE_OUTER_BOUND('',#478,.T.);
#323=FACE_OUTER_BOUND('',#484,.T.);
#324=FACE_OUTER_BOUND('',#485,.T.);
#325=FACE_OUTER_BOUND('',#486,.T.);
#326=FACE_OUTER_BOUND('',#487,.T.);
#327=FACE_OUTER_BOUND('',#488,.T.);
#328=FACE_OUTER_BOUND('',#489,.T.);
#329=FACE_OUTER_BOUND('',#490,.T.);
#330=FACE_OUTER_BOUND('',#491,.T.);
#331=FACE_OUTER_BOUND('',#492,.T.);
#332=FACE_OUTER_BOUND('',#493,.T.);
#333=FACE_OUTER_BOUND('',#495,.T.);
#334=FACE_OUTER_BOUND('',#496,.T.);
#335=FACE_OUTER_BOUND('',#498,.T.);
#336=FACE_OUTER_BOUND('',#500,.T.);
#337=FACE_OUTER_BOUND('',#501,.T.);
#338=FACE_OUTER_BOUND('',#502,.T.);
#339=FACE_OUTER_BOUND('',#503,.T.);
#340=FACE_OUTER_BOUND('',#505,.T.);
#341=FACE_OUTER_BOUND('',#506,.T.);
#342=FACE_OUTER_BOUND('',#507,.T.);
#343=FACE_OUTER_BOUND('',#508,.T.);
#344=FACE_OUTER_BOUND('',#509,.T.);
#345=FACE_OUTER_BOUND('',#510,.T.);
#346=FACE_OUTER_BOUND('',#511,.T.);
#347=FACE_OUTER_BOUND('',#512,.T.);
#348=FACE_OUTER_BOUND('',#513,.T.);
#349=FACE_OUTER_BOUND('',#514,.T.);
#350=FACE_OUTER_BOUND('',#515,.T.);
#351=FACE_OUTER_BOUND('',#516,.T.);
#352=FACE_OUTER_BOUND('',#517,.T.);
#353=FACE_OUTER_BOUND('',#523,.T.);
#354=FACE_OUTER_BOUND('',#529,.T.);
#355=FACE_OUTER_BOUND('',#530,.T.);
#356=FACE_OUTER_BOUND('',#531,.T.);
#357=FACE_OUTER_BOUND('',#532,.T.);
#358=FACE_OUTER_BOUND('',#533,.T.);
#359=FACE_OUTER_BOUND('',#534,.T.);
#360=FACE_OUTER_BOUND('',#535,.T.);
#361=FACE_OUTER_BOUND('',#537,.T.);
#362=FACE_OUTER_BOUND('',#538,.T.);
#363=FACE_OUTER_BOUND('',#539,.T.);
#364=FACE_OUTER_BOUND('',#540,.T.);
#365=FACE_OUTER_BOUND('',#541,.T.);
#366=FACE_OUTER_BOUND('',#542,.T.);
#367=FACE_OUTER_BOUND('',#543,.T.);
#368=FACE_OUTER_BOUND('',#544,.T.);
#369=FACE_OUTER_BOUND('',#545,.T.);
#370=FACE_OUTER_BOUND('',#546,.T.);
#371=FACE_OUTER_BOUND('',#547,.T.);
#372=FACE_OUTER_BOUND('',#548,.T.);
#373=FACE_OUTER_BOUND('',#549,.T.);
#374=FACE_OUTER_BOUND('',#550,.T.);
#375=FACE_OUTER_BOUND('',#551,.T.);
#376=FACE_OUTER_BOUND('',#552,.T.);
#377=FACE_OUTER_BOUND('',#553,.T.);
#378=FACE_OUTER_BOUND('',#554,.T.);
#379=FACE_OUTER_BOUND('',#555,.T.);
#380=FACE_OUTER_BOUND('',#556,.T.);
#381=FACE_OUTER_BOUND('',#557,.T.);
#382=FACE_OUTER_BOUND('',#558,.T.);
#383=FACE_OUTER_BOUND('',#559,.T.);
#384=FACE_OUTER_BOUND('',#560,.T.);
#385=FACE_OUTER_BOUND('',#561,.T.);
#386=FACE_OUTER_BOUND('',#562,.T.);
#387=FACE_OUTER_BOUND('',#563,.T.);
#388=FACE_OUTER_BOUND('',#564,.T.);
#389=FACE_OUTER_BOUND('',#565,.T.);
#390=FACE_OUTER_BOUND('',#566,.T.);
#391=FACE_OUTER_BOUND('',#567,.T.);
#392=FACE_OUTER_BOUND('',#568,.T.);
#393=FACE_OUTER_BOUND('',#569,.T.);
#394=FACE_OUTER_BOUND('',#570,.T.);
#395=FACE_OUTER_BOUND('',#571,.T.);
#396=FACE_OUTER_BOUND('',#572,.T.);
#397=FACE_OUTER_BOUND('',#573,.T.);
#398=FACE_OUTER_BOUND('',#574,.T.);
#399=FACE_OUTER_BOUND('',#575,.T.);
#400=FACE_OUTER_BOUND('',#576,.T.);
#401=FACE_OUTER_BOUND('',#577,.T.);
#402=FACE_OUTER_BOUND('',#578,.T.);
#403=FACE_OUTER_BOUND('',#579,.T.);
#404=FACE_OUTER_BOUND('',#580,.T.);
#405=FACE_OUTER_BOUND('',#581,.T.);
#406=FACE_OUTER_BOUND('',#582,.T.);
#407=FACE_OUTER_BOUND('',#583,.T.);
#408=FACE_OUTER_BOUND('',#584,.T.);
#409=FACE_OUTER_BOUND('',#585,.T.);
#410=FACE_OUTER_BOUND('',#586,.T.);
#411=FACE_OUTER_BOUND('',#587,.T.);
#412=FACE_OUTER_BOUND('',#588,.T.);
#413=FACE_OUTER_BOUND('',#589,.T.);
#414=FACE_OUTER_BOUND('',#590,.T.);
#415=FACE_OUTER_BOUND('',#591,.T.);
#416=FACE_OUTER_BOUND('',#592,.T.);
#417=FACE_OUTER_BOUND('',#593,.T.);
#418=FACE_OUTER_BOUND('',#594,.T.);
#419=FACE_OUTER_BOUND('',#595,.T.);
#420=FACE_OUTER_BOUND('',#596,.T.);
#421=FACE_OUTER_BOUND('',#597,.T.);
#422=FACE_OUTER_BOUND('',#598,.T.);
#423=FACE_OUTER_BOUND('',#599,.T.);
#424=FACE_OUTER_BOUND('',#600,.T.);
#425=FACE_OUTER_BOUND('',#601,.T.);
#426=FACE_OUTER_BOUND('',#602,.T.);
#427=FACE_OUTER_BOUND('',#603,.T.);
#428=FACE_OUTER_BOUND('',#604,.T.);
#429=FACE_OUTER_BOUND('',#610,.T.);
#430=FACE_OUTER_BOUND('',#611,.T.);
#431=FACE_OUTER_BOUND('',#612,.T.);
#432=FACE_OUTER_BOUND('',#613,.T.);
#433=FACE_OUTER_BOUND('',#614,.T.);
#434=FACE_OUTER_BOUND('',#615,.T.);
#435=FACE_OUTER_BOUND('',#616,.T.);
#436=FACE_OUTER_BOUND('',#617,.T.);
#437=FACE_OUTER_BOUND('',#618,.T.);
#438=FACE_OUTER_BOUND('',#619,.T.);
#439=FACE_OUTER_BOUND('',#622,.T.);
#440=FACE_OUTER_BOUND('',#623,.T.);
#441=FACE_OUTER_BOUND('',#626,.T.);
#442=FACE_OUTER_BOUND('',#627,.T.);
#443=FACE_OUTER_BOUND('',#628,.T.);
#444=FACE_OUTER_BOUND('',#629,.T.);
#445=FACE_OUTER_BOUND('',#630,.T.);
#446=FACE_OUTER_BOUND('',#631,.T.);
#447=FACE_OUTER_BOUND('',#633,.T.);
#448=FACE_OUTER_BOUND('',#635,.T.);
#449=FACE_OUTER_BOUND('',#637,.T.);
#450=FACE_OUTER_BOUND('',#638,.T.);
#451=FACE_OUTER_BOUND('',#639,.T.);
#452=FACE_OUTER_BOUND('',#640,.T.);
#453=FACE_OUTER_BOUND('',#641,.T.);
#454=FACE_OUTER_BOUND('',#642,.T.);
#455=FACE_OUTER_BOUND('',#643,.T.);
#456=FACE_OUTER_BOUND('',#644,.T.);
#457=FACE_OUTER_BOUND('',#645,.T.);
#458=FACE_OUTER_BOUND('',#646,.T.);
#459=FACE_OUTER_BOUND('',#647,.T.);
#460=FACE_OUTER_BOUND('',#648,.T.);
#461=FACE_OUTER_BOUND('',#649,.T.);
#462=EDGE_LOOP('',(#1621,#1622,#1623));
#463=EDGE_LOOP('',(#1624,#1625,#1626,#1627));
#464=EDGE_LOOP('',(#1628,#1629,#1630));
#465=EDGE_LOOP('',(#1631,#1632,#1633,#1634));
#466=EDGE_LOOP('',(#1635,#1636,#1637));
#467=EDGE_LOOP('',(#1638,#1639,#1640,#1641));
#468=EDGE_LOOP('',(#1642,#1643,#1644));
#469=EDGE_LOOP('',(#1645,#1646,#1647,#1648));
#470=EDGE_LOOP('',(#1649,#1650,#1651,#1652,#1653,#1654));
#471=EDGE_LOOP('',(#1655,#1656,#1657,#1658,#1659,#1660,#1661,#1662));
#472=EDGE_LOOP('',(#1663,#1664,#1665,#1666,#1667,#1668,#1669));
#473=EDGE_LOOP('',(#1670,#1671,#1672,#1673));
#474=EDGE_LOOP('',(#1674));
#475=EDGE_LOOP('',(#1675,#1676,#1677,#1678));
#476=EDGE_LOOP('',(#1679));
#477=EDGE_LOOP('',(#1680,#1681,#1682,#1683));
#478=EDGE_LOOP('',(#1684,#1685,#1686,#1687));
#479=EDGE_LOOP('',(#1688));
#480=EDGE_LOOP('',(#1689));
#481=EDGE_LOOP('',(#1690));
#482=EDGE_LOOP('',(#1691));
#483=EDGE_LOOP('',(#1692));
#484=EDGE_LOOP('',(#1693,#1694,#1695,#1696));
#485=EDGE_LOOP('',(#1697,#1698,#1699,#1700));
#486=EDGE_LOOP('',(#1701,#1702));
#487=EDGE_LOOP('',(#1703,#1704));
#488=EDGE_LOOP('',(#1705,#1706,#1707,#1708,#1709,#1710));
#489=EDGE_LOOP('',(#1711,#1712,#1713,#1714));
#490=EDGE_LOOP('',(#1715,#1716,#1717,#1718));
#491=EDGE_LOOP('',(#1719,#1720,#1721,#1722));
#492=EDGE_LOOP('',(#1723,#1724,#1725,#1726));
#493=EDGE_LOOP('',(#1727));
#494=EDGE_LOOP('',(#1728));
#495=EDGE_LOOP('',(#1729));
#496=EDGE_LOOP('',(#1730));
#497=EDGE_LOOP('',(#1731));
#498=EDGE_LOOP('',(#1732));
#499=EDGE_LOOP('',(#1733));
#500=EDGE_LOOP('',(#1734));
#501=EDGE_LOOP('',(#1735,#1736,#1737,#1738));
#502=EDGE_LOOP('',(#1739,#1740,#1741,#1742));
#503=EDGE_LOOP('',(#1743));
#504=EDGE_LOOP('',(#1744));
#505=EDGE_LOOP('',(#1745));
#506=EDGE_LOOP('',(#1746));
#507=EDGE_LOOP('',(#1747,#1748,#1749,#1750,#1751));
#508=EDGE_LOOP('',(#1752,#1753,#1754));
#509=EDGE_LOOP('',(#1755,#1756));
#510=EDGE_LOOP('',(#1757,#1758,#1759,#1760,#1761));
#511=EDGE_LOOP('',(#1762,#1763,#1764));
#512=EDGE_LOOP('',(#1765,#1766,#1767,#1768));
#513=EDGE_LOOP('',(#1769,#1770,#1771,#1772));
#514=EDGE_LOOP('',(#1773,#1774,#1775,#1776));
#515=EDGE_LOOP('',(#1777,#1778,#1779,#1780));
#516=EDGE_LOOP('',(#1781,#1782,#1783,#1784));
#517=EDGE_LOOP('',(#1785,#1786,#1787,#1788));
#518=EDGE_LOOP('',(#1789));
#519=EDGE_LOOP('',(#1790));
#520=EDGE_LOOP('',(#1791));
#521=EDGE_LOOP('',(#1792));
#522=EDGE_LOOP('',(#1793));
#523=EDGE_LOOP('',(#1794,#1795,#1796,#1797));
#524=EDGE_LOOP('',(#1798));
#525=EDGE_LOOP('',(#1799));
#526=EDGE_LOOP('',(#1800));
#527=EDGE_LOOP('',(#1801));
#528=EDGE_LOOP('',(#1802));
#529=EDGE_LOOP('',(#1803,#1804,#1805,#1806));
#530=EDGE_LOOP('',(#1807,#1808,#1809,#1810));
#531=EDGE_LOOP('',(#1811,#1812,#1813,#1814));
#532=EDGE_LOOP('',(#1815,#1816,#1817,#1818));
#533=EDGE_LOOP('',(#1819,#1820,#1821,#1822));
#534=EDGE_LOOP('',(#1823,#1824,#1825,#1826));
#535=EDGE_LOOP('',(#1827,#1828,#1829,#1830));
#536=EDGE_LOOP('',(#1831));
#537=EDGE_LOOP('',(#1832,#1833,#1834,#1835));
#538=EDGE_LOOP('',(#1836,#1837,#1838,#1839));
#539=EDGE_LOOP('',(#1840,#1841,#1842,#1843));
#540=EDGE_LOOP('',(#1844));
#541=EDGE_LOOP('',(#1845,#1846,#1847,#1848));
#542=EDGE_LOOP('',(#1849,#1850,#1851,#1852));
#543=EDGE_LOOP('',(#1853,#1854,#1855,#1856));
#544=EDGE_LOOP('',(#1857,#1858,#1859,#1860));
#545=EDGE_LOOP('',(#1861,#1862,#1863,#1864));
#546=EDGE_LOOP('',(#1865,#1866,#1867,#1868));
#547=EDGE_LOOP('',(#1869,#1870,#1871,#1872));
#548=EDGE_LOOP('',(#1873,#1874,#1875,#1876));
#549=EDGE_LOOP('',(#1877,#1878,#1879,#1880));
#550=EDGE_LOOP('',(#1881,#1882,#1883,#1884));
#551=EDGE_LOOP('',(#1885,#1886,#1887,#1888));
#552=EDGE_LOOP('',(#1889,#1890,#1891,#1892));
#553=EDGE_LOOP('',(#1893,#1894,#1895,#1896));
#554=EDGE_LOOP('',(#1897,#1898,#1899,#1900));
#555=EDGE_LOOP('',(#1901,#1902,#1903,#1904));
#556=EDGE_LOOP('',(#1905,#1906,#1907,#1908));
#557=EDGE_LOOP('',(#1909,#1910,#1911,#1912));
#558=EDGE_LOOP('',(#1913,#1914,#1915,#1916));
#559=EDGE_LOOP('',(#1917,#1918,#1919,#1920));
#560=EDGE_LOOP('',(#1921,#1922,#1923,#1924));
#561=EDGE_LOOP('',(#1925,#1926,#1927,#1928));
#562=EDGE_LOOP('',(#1929,#1930,#1931,#1932));
#563=EDGE_LOOP('',(#1933,#1934,#1935,#1936));
#564=EDGE_LOOP('',(#1937,#1938,#1939,#1940));
#565=EDGE_LOOP('',(#1941,#1942,#1943,#1944));
#566=EDGE_LOOP('',(#1945,#1946,#1947,#1948));
#567=EDGE_LOOP('',(#1949,#1950,#1951,#1952));
#568=EDGE_LOOP('',(#1953,#1954,#1955,#1956));
#569=EDGE_LOOP('',(#1957,#1958,#1959,#1960));
#570=EDGE_LOOP('',(#1961,#1962,#1963,#1964));
#571=EDGE_LOOP('',(#1965,#1966,#1967,#1968));
#572=EDGE_LOOP('',(#1969,#1970,#1971,#1972));
#573=EDGE_LOOP('',(#1973,#1974,#1975,#1976));
#574=EDGE_LOOP('',(#1977,#1978,#1979,#1980));
#575=EDGE_LOOP('',(#1981,#1982,#1983,#1984));
#576=EDGE_LOOP('',(#1985,#1986,#1987,#1988));
#577=EDGE_LOOP('',(#1989,#1990,#1991,#1992));
#578=EDGE_LOOP('',(#1993,#1994,#1995,#1996));
#579=EDGE_LOOP('',(#1997,#1998,#1999,#2000));
#580=EDGE_LOOP('',(#2001,#2002,#2003,#2004));
#581=EDGE_LOOP('',(#2005,#2006,#2007,#2008));
#582=EDGE_LOOP('',(#2009,#2010,#2011,#2012));
#583=EDGE_LOOP('',(#2013,#2014,#2015,#2016));
#584=EDGE_LOOP('',(#2017,#2018,#2019,#2020));
#585=EDGE_LOOP('',(#2021,#2022,#2023,#2024));
#586=EDGE_LOOP('',(#2025,#2026,#2027,#2028));
#587=EDGE_LOOP('',(#2029,#2030,#2031,#2032));
#588=EDGE_LOOP('',(#2033,#2034,#2035,#2036));
#589=EDGE_LOOP('',(#2037,#2038,#2039,#2040));
#590=EDGE_LOOP('',(#2041,#2042,#2043,#2044));
#591=EDGE_LOOP('',(#2045,#2046,#2047,#2048));
#592=EDGE_LOOP('',(#2049,#2050,#2051,#2052));
#593=EDGE_LOOP('',(#2053,#2054,#2055,#2056));
#594=EDGE_LOOP('',(#2057,#2058,#2059,#2060));
#595=EDGE_LOOP('',(#2061,#2062,#2063,#2064));
#596=EDGE_LOOP('',(#2065,#2066,#2067,#2068));
#597=EDGE_LOOP('',(#2069,#2070,#2071,#2072));
#598=EDGE_LOOP('',(#2073,#2074,#2075,#2076));
#599=EDGE_LOOP('',(#2077,#2078,#2079,#2080));
#600=EDGE_LOOP('',(#2081,#2082,#2083,#2084));
#601=EDGE_LOOP('',(#2085,#2086,#2087,#2088));
#602=EDGE_LOOP('',(#2089,#2090,#2091,#2092));
#603=EDGE_LOOP('',(#2093,#2094,#2095,#2096));
#604=EDGE_LOOP('',(#2097,#2098,#2099,#2100));
#605=EDGE_LOOP('',(#2101,#2102,#2103,#2104));
#606=EDGE_LOOP('',(#2105));
#607=EDGE_LOOP('',(#2106));
#608=EDGE_LOOP('',(#2107));
#609=EDGE_LOOP('',(#2108));
#610=EDGE_LOOP('',(#2109,#2110,#2111,#2112,#2113,#2114,#2115,#2116));
#611=EDGE_LOOP('',(#2117,#2118,#2119,#2120,#2121,#2122,#2123,#2124));
#612=EDGE_LOOP('',(#2125,#2126,#2127,#2128));
#613=EDGE_LOOP('',(#2129,#2130,#2131,#2132));
#614=EDGE_LOOP('',(#2133,#2134,#2135,#2136));
#615=EDGE_LOOP('',(#2137,#2138,#2139,#2140));
#616=EDGE_LOOP('',(#2141,#2142,#2143,#2144));
#617=EDGE_LOOP('',(#2145,#2146,#2147,#2148));
#618=EDGE_LOOP('',(#2149,#2150,#2151,#2152));
#619=EDGE_LOOP('',(#2153,#2154,#2155,#2156));
#620=EDGE_LOOP('',(#2157));
#621=EDGE_LOOP('',(#2158));
#622=EDGE_LOOP('',(#2159,#2160,#2161,#2162));
#623=EDGE_LOOP('',(#2163,#2164,#2165,#2166));
#624=EDGE_LOOP('',(#2167));
#625=EDGE_LOOP('',(#2168));
#626=EDGE_LOOP('',(#2169,#2170,#2171,#2172,#2173,#2174,#2175,#2176));
#627=EDGE_LOOP('',(#2177,#2178,#2179,#2180));
#628=EDGE_LOOP('',(#2181,#2182,#2183,#2184));
#629=EDGE_LOOP('',(#2185,#2186,#2187,#2188));
#630=EDGE_LOOP('',(#2189,#2190,#2191,#2192));
#631=EDGE_LOOP('',(#2193));
#632=EDGE_LOOP('',(#2194));
#633=EDGE_LOOP('',(#2195));
#634=EDGE_LOOP('',(#2196,#2197,#2198,#2199,#2200,#2201));
#635=EDGE_LOOP('',(#2202));
#636=EDGE_LOOP('',(#2203));
#637=EDGE_LOOP('',(#2204));
#638=EDGE_LOOP('',(#2205,#2206,#2207,#2208,#2209));
#639=EDGE_LOOP('',(#2210,#2211,#2212,#2213,#2214));
#640=EDGE_LOOP('',(#2215,#2216,#2217,#2218,#2219));
#641=EDGE_LOOP('',(#2220,#2221,#2222,#2223,#2224));
#642=EDGE_LOOP('',(#2225,#2226,#2227,#2228,#2229));
#643=EDGE_LOOP('',(#2230,#2231,#2232,#2233,#2234));
#644=EDGE_LOOP('',(#2235,#2236,#2237));
#645=EDGE_LOOP('',(#2238,#2239,#2240));
#646=EDGE_LOOP('',(#2241,#2242,#2243));
#647=EDGE_LOOP('',(#2244,#2245,#2246));
#648=EDGE_LOOP('',(#2247,#2248,#2249));
#649=EDGE_LOOP('',(#2250,#2251,#2252));
#650=CIRCLE('',#2537,2.);
#651=CIRCLE('',#2539,2.);
#652=CIRCLE('',#2541,2.);
#653=CIRCLE('',#2543,2.);
#654=CIRCLE('',#2545,2.);
#655=CIRCLE('',#2547,2.);
#656=CIRCLE('',#2549,2.);
#657=CIRCLE('',#2551,2.);
#658=CIRCLE('',#2555,4.);
#659=CIRCLE('',#2558,4.);
#660=CIRCLE('',#2559,4.);
#661=CIRCLE('',#2561,4.);
#662=CIRCLE('',#2562,4.);
#663=CIRCLE('',#2574,5.);
#664=CIRCLE('',#2575,5.);
#665=CIRCLE('',#2577,6.);
#666=CIRCLE('',#2578,6.);
#667=CIRCLE('',#2580,2.5);
#668=CIRCLE('',#2581,2.5);
#669=CIRCLE('',#2583,4.);
#670=CIRCLE('',#2584,4.);
#671=CIRCLE('',#2592,2.5);
#672=CIRCLE('',#2593,2.5);
#673=CIRCLE('',#2595,4.);
#674=CIRCLE('',#2596,4.);
#675=CIRCLE('',#2601,0.500000000000003);
#676=CIRCLE('',#2602,0.499999999999999);
#677=CIRCLE('',#2604,0.499999999999999);
#678=CIRCLE('',#2606,0.500000000000003);
#679=CIRCLE('',#2610,2.15);
#680=CIRCLE('',#2611,2.15);
#681=CIRCLE('',#2613,2.15);
#682=CIRCLE('',#2614,2.15);
#683=CIRCLE('',#2616,2.15);
#684=CIRCLE('',#2617,2.15);
#685=CIRCLE('',#2619,2.15);
#686=CIRCLE('',#2620,2.15);
#687=CIRCLE('',#2622,7.);
#688=CIRCLE('',#2623,7.);
#689=CIRCLE('',#2632,6.5);
#690=CIRCLE('',#2633,6.5);
#691=CIRCLE('',#2635,8.);
#692=CIRCLE('',#2636,8.);
#693=CIRCLE('',#2638,8.);
#694=CIRCLE('',#2640,8.);
#695=CIRCLE('',#2647,0.999999999999999);
#696=CIRCLE('',#2648,8.00000000000001);
#697=CIRCLE('',#2649,0.999999999999999);
#698=CIRCLE('',#2651,0.999999999999999);
#699=CIRCLE('',#2652,8.);
#700=CIRCLE('',#2653,0.999999999999999);
#701=CIRCLE('',#2657,0.999999999999999);
#702=CIRCLE('',#2658,8.00000000000001);
#703=CIRCLE('',#2659,0.999999999999999);
#704=CIRCLE('',#2661,0.999999999999999);
#705=CIRCLE('',#2662,8.);
#706=CIRCLE('',#2663,0.999999999999999);
#707=CIRCLE('',#2667,0.999999999999999);
#708=CIRCLE('',#2668,8.00000000000001);
#709=CIRCLE('',#2669,0.999999999999999);
#710=CIRCLE('',#2671,0.999999999999999);
#711=CIRCLE('',#2672,8.);
#712=CIRCLE('',#2673,0.999999999999999);
#713=CIRCLE('',#2677,0.999999999999999);
#714=CIRCLE('',#2678,8.00000000000001);
#715=CIRCLE('',#2679,0.999999999999999);
#716=CIRCLE('',#2681,0.999999999999999);
#717=CIRCLE('',#2682,8.);
#718=CIRCLE('',#2683,0.999999999999999);
#719=CIRCLE('',#2687,0.999999999999999);
#720=CIRCLE('',#2688,8.00000000000001);
#721=CIRCLE('',#2689,0.999999999999999);
#722=CIRCLE('',#2691,0.999999999999999);
#723=CIRCLE('',#2692,8.);
#724=CIRCLE('',#2693,0.999999999999999);
#725=CIRCLE('',#2697,0.999999999999999);
#726=CIRCLE('',#2698,8.00000000000001);
#727=CIRCLE('',#2699,0.999999999999999);
#728=CIRCLE('',#2701,0.999999999999999);
#729=CIRCLE('',#2702,8.);
#730=CIRCLE('',#2703,0.999999999999999);
#731=CIRCLE('',#2707,0.999999999999999);
#732=CIRCLE('',#2708,8.00000000000001);
#733=CIRCLE('',#2709,0.999999999999999);
#734=CIRCLE('',#2711,0.999999999999999);
#735=CIRCLE('',#2712,8.);
#736=CIRCLE('',#2713,0.999999999999999);
#737=CIRCLE('',#2717,0.999999999999999);
#738=CIRCLE('',#2718,8.00000000000001);
#739=CIRCLE('',#2719,0.999999999999999);
#740=CIRCLE('',#2721,0.999999999999999);
#741=CIRCLE('',#2722,8.);
#742=CIRCLE('',#2723,0.999999999999999);
#743=CIRCLE('',#2727,0.999999999999999);
#744=CIRCLE('',#2728,8.00000000000001);
#745=CIRCLE('',#2729,0.999999999999999);
#746=CIRCLE('',#2731,0.999999999999999);
#747=CIRCLE('',#2732,8.);
#748=CIRCLE('',#2733,0.999999999999999);
#749=CIRCLE('',#2737,0.999999999999999);
#750=CIRCLE('',#2738,8.00000000000001);
#751=CIRCLE('',#2739,0.999999999999999);
#752=CIRCLE('',#2741,0.999999999999999);
#753=CIRCLE('',#2742,8.);
#754=CIRCLE('',#2743,0.999999999999999);
#755=CIRCLE('',#2747,0.999999999999999);
#756=CIRCLE('',#2748,8.00000000000001);
#757=CIRCLE('',#2749,0.999999999999999);
#758=CIRCLE('',#2751,0.999999999999999);
#759=CIRCLE('',#2752,8.);
#760=CIRCLE('',#2753,0.999999999999999);
#761=CIRCLE('',#2757,0.999999999999999);
#762=CIRCLE('',#2758,8.00000000000001);
#763=CIRCLE('',#2759,0.999999999999999);
#764=CIRCLE('',#2761,0.999999999999999);
#765=CIRCLE('',#2762,8.);
#766=CIRCLE('',#2763,0.999999999999999);
#767=CIRCLE('',#2767,0.999999999999999);
#768=CIRCLE('',#2768,8.00000000000001);
#769=CIRCLE('',#2769,0.999999999999999);
#770=CIRCLE('',#2771,0.999999999999999);
#771=CIRCLE('',#2772,8.);
#772=CIRCLE('',#2773,0.999999999999999);
#773=CIRCLE('',#2778,2.15);
#774=CIRCLE('',#2779,0.2);
#775=CIRCLE('',#2780,2.2);
#776=CIRCLE('',#2782,2.15);
#777=CIRCLE('',#2783,0.2);
#778=CIRCLE('',#2784,2.2);
#779=CIRCLE('',#2786,2.15);
#780=CIRCLE('',#2787,0.2);
#781=CIRCLE('',#2788,2.2);
#782=CIRCLE('',#2790,2.15);
#783=CIRCLE('',#2791,0.2);
#784=CIRCLE('',#2792,2.2);
#785=CIRCLE('',#2794,2.15);
#786=CIRCLE('',#2796,2.15);
#787=CIRCLE('',#2798,2.15);
#788=CIRCLE('',#2800,2.15);
#789=CIRCLE('',#2818,1.25);
#790=CIRCLE('',#2819,1.25);
#791=CIRCLE('',#2820,1.25);
#792=CIRCLE('',#2821,1.25);
#793=CIRCLE('',#2822,1.25);
#794=CIRCLE('',#2823,1.25);
#795=CIRCLE('',#2825,2.2);
#796=CIRCLE('',#2826,0.2);
#797=CIRCLE('',#2827,2.);
#798=CIRCLE('',#2829,2.);
#799=CIRCLE('',#2830,1.61);
#800=CIRCLE('',#2833,3.8);
#801=CIRCLE('',#2834,3.8);
#802=CIRCLE('',#2836,1.9);
#803=LINE('',#3685,#959);
#804=LINE('',#3689,#960);
#805=LINE('',#3694,#961);
#806=LINE('',#3698,#962);
#807=LINE('',#3703,#963);
#808=LINE('',#3707,#964);
#809=LINE('',#3712,#965);
#810=LINE('',#3716,#966);
#811=LINE('',#3725,#967);
#812=LINE('',#3733,#968);
#813=LINE('',#3735,#969);
#814=LINE('',#3736,#970);
#815=LINE('',#3741,#971);
#816=LINE('',#3744,#972);
#817=LINE('',#3745,#973);
#818=LINE('',#3749,#974);
#819=LINE('',#3751,#975);
#820=LINE('',#3753,#976);
#821=LINE('',#3754,#977);
#822=LINE('',#3758,#978);
#823=LINE('',#3760,#979);
#824=LINE('',#3762,#980);
#825=LINE('',#3763,#981);
#826=LINE('',#3765,#982);
#827=LINE('',#3766,#983);
#828=LINE('',#3768,#984);
#829=LINE('',#3770,#985);
#830=LINE('',#3773,#986);
#831=LINE('',#3775,#987);
#832=LINE('',#3782,#988);
#833=LINE('',#3788,#989);
#834=LINE('',#3794,#990);
#835=LINE('',#3800,#991);
#836=LINE('',#3812,#992);
#837=LINE('',#3818,#993);
#838=LINE('',#5658,#994);
#839=LINE('',#7093,#995);
#840=LINE('',#7099,#996);
#841=LINE('',#7105,#997);
#842=LINE('',#7111,#998);
#843=LINE('',#7117,#999);
#844=LINE('',#7122,#1000);
#845=LINE('',#7124,#1001);
#846=LINE('',#7126,#1002);
#847=LINE('',#7127,#1003);
#848=LINE('',#7131,#1004);
#849=LINE('',#7133,#1005);
#850=LINE('',#7135,#1006);
#851=LINE('',#7136,#1007);
#852=LINE('',#7138,#1008);
#853=LINE('',#7139,#1009);
#854=LINE('',#7141,#1010);
#855=LINE('',#7143,#1011);
#856=LINE('',#7150,#1012);
#857=LINE('',#7157,#1013);
#858=LINE('',#7160,#1014);
#859=LINE('',#7165,#1015);
#860=LINE('',#7166,#1016);
#861=LINE('',#7169,#1017);
#862=LINE('',#7172,#1018);
#863=LINE('',#7174,#1019);
#864=LINE('',#7176,#1020);
#865=LINE('',#7193,#1021);
#866=LINE('',#7195,#1022);
#867=LINE('',#7209,#1023);
#868=LINE('',#7211,#1024);
#869=LINE('',#7225,#1025);
#870=LINE('',#7227,#1026);
#871=LINE('',#7241,#1027);
#872=LINE('',#7243,#1028);
#873=LINE('',#7257,#1029);
#874=LINE('',#7259,#1030);
#875=LINE('',#7273,#1031);
#876=LINE('',#7275,#1032);
#877=LINE('',#7289,#1033);
#878=LINE('',#7291,#1034);
#879=LINE('',#7305,#1035);
#880=LINE('',#7307,#1036);
#881=LINE('',#7321,#1037);
#882=LINE('',#7323,#1038);
#883=LINE('',#7337,#1039);
#884=LINE('',#7339,#1040);
#885=LINE('',#7353,#1041);
#886=LINE('',#7355,#1042);
#887=LINE('',#7369,#1043);
#888=LINE('',#7371,#1044);
#889=LINE('',#7385,#1045);
#890=LINE('',#7387,#1046);
#891=LINE('',#7416,#1047);
#892=LINE('',#7420,#1048);
#893=LINE('',#7424,#1049);
#894=LINE('',#7428,#1050);
#895=LINE('',#7432,#1051);
#896=LINE('',#7434,#1052);
#897=LINE('',#7436,#1053);
#898=LINE('',#7437,#1054);
#899=LINE('',#7441,#1055);
#900=LINE('',#7443,#1056);
#901=LINE('',#7445,#1057);
#902=LINE('',#7446,#1058);
#903=LINE('',#7450,#1059);
#904=LINE('',#7452,#1060);
#905=LINE('',#7454,#1061);
#906=LINE('',#7455,#1062);
#907=LINE('',#7458,#1063);
#908=LINE('',#7460,#1064);
#909=LINE('',#7462,#1065);
#910=LINE('',#7463,#1066);
#911=LINE('',#7466,#1067);
#912=LINE('',#7467,#1068);
#913=LINE('',#7468,#1069);
#914=LINE('',#7470,#1070);
#915=LINE('',#7471,#1071);
#916=LINE('',#7474,#1072);
#917=LINE('',#7475,#1073);
#918=LINE('',#7476,#1074);
#919=LINE('',#7478,#1075);
#920=LINE('',#7479,#1076);
#921=LINE('',#7482,#1077);
#922=LINE('',#7484,#1078);
#923=LINE('',#7485,#1079);
#924=LINE('',#7488,#1080);
#925=LINE('',#7489,#1081);
#926=LINE('',#7492,#1082);
#927=LINE('',#7493,#1083);
#928=LINE('',#7495,#1084);
#929=LINE('',#7499,#1085);
#930=LINE('',#7502,#1086);
#931=LINE('',#7508,#1087);
#932=LINE('',#7530,#1088);
#933=LINE('',#7533,#1089);
#934=LINE('',#7538,#1090);
#935=LINE('',#7546,#1091);
#936=LINE('',#7548,#1092);
#937=LINE('',#7550,#1093);
#938=LINE('',#7552,#1094);
#939=LINE('',#7554,#1095);
#940=LINE('',#7555,#1096);
#941=LINE('',#7560,#1097);
#942=LINE('',#7562,#1098);
#943=LINE('',#7563,#1099);
#944=LINE('',#7564,#1100);
#945=LINE('',#7566,#1101);
#946=LINE('',#7568,#1102);
#947=LINE('',#7569,#1103);
#948=LINE('',#7571,#1104);
#949=LINE('',#7573,#1105);
#950=LINE('',#7574,#1106);
#951=LINE('',#7576,#1107);
#952=LINE('',#7578,#1108);
#953=LINE('',#7579,#1109);
#954=LINE('',#7581,#1110);
#955=LINE('',#7583,#1111);
#956=LINE('',#7584,#1112);
#957=LINE('',#7586,#1113);
#958=LINE('',#7587,#1114);
#959=VECTOR('',#2870,2.);
#960=VECTOR('',#2875,2.);
#961=VECTOR('',#2880,2.);
#962=VECTOR('',#2885,2.);
#963=VECTOR('',#2890,2.);
#964=VECTOR('',#2895,2.);
#965=VECTOR('',#2900,2.);
#966=VECTOR('',#2905,2.);
#967=VECTOR('',#2914,4.);
#968=VECTOR('',#2923,4.);
#969=VECTOR('',#2926,1000.);
#970=VECTOR('',#2927,1000.);
#971=VECTOR('',#2932,4.);
#972=VECTOR('',#2935,1000.);
#973=VECTOR('',#2936,1000.);
#974=VECTOR('',#2939,1000.);
#975=VECTOR('',#2940,1000.);
#976=VECTOR('',#2941,1000.);
#977=VECTOR('',#2942,1000.);
#978=VECTOR('',#2945,1000.);
#979=VECTOR('',#2946,1000.);
#980=VECTOR('',#2947,1000.);
#981=VECTOR('',#2948,1000.);
#982=VECTOR('',#2951,1000.);
#983=VECTOR('',#2952,1000.);
#984=VECTOR('',#2955,1000.);
#985=VECTOR('',#2958,1000.);
#986=VECTOR('',#2963,1000.);
#987=VECTOR('',#2966,1000.);
#988=VECTOR('',#2975,5.);
#989=VECTOR('',#2982,6.);
#990=VECTOR('',#2989,2.5);
#991=VECTOR('',#2996,4.);
#992=VECTOR('',#3015,2.5);
#993=VECTOR('',#3022,4.);
#994=VECTOR('',#3039,1000.);
#995=VECTOR('',#3054,2.15);
#996=VECTOR('',#3061,2.15);
#997=VECTOR('',#3068,2.15);
#998=VECTOR('',#3075,2.15);
#999=VECTOR('',#3082,7.);
#1000=VECTOR('',#3087,1000.);
#1001=VECTOR('',#3088,1000.);
#1002=VECTOR('',#3089,1000.);
#1003=VECTOR('',#3090,1000.);
#1004=VECTOR('',#3093,1000.);
#1005=VECTOR('',#3094,1000.);
#1006=VECTOR('',#3095,1000.);
#1007=VECTOR('',#3096,1000.);
#1008=VECTOR('',#3099,1000.);
#1009=VECTOR('',#3100,1000.);
#1010=VECTOR('',#3103,1000.);
#1011=VECTOR('',#3106,1000.);
#1012=VECTOR('',#3115,6.5);
#1013=VECTOR('',#3122,1000.);
#1014=VECTOR('',#3125,1000.);
#1015=VECTOR('',#3130,1000.);
#1016=VECTOR('',#3131,1000.);
#1017=VECTOR('',#3134,1000.);
#1018=VECTOR('',#3137,1000.);
#1019=VECTOR('',#3140,1000.);
#1020=VECTOR('',#3143,1000.);
#1021=VECTOR('',#3168,0.999999999999999);
#1022=VECTOR('',#3171,0.999999999999999);
#1023=VECTOR('',#3190,0.999999999999999);
#1024=VECTOR('',#3193,0.999999999999999);
#1025=VECTOR('',#3212,0.999999999999999);
#1026=VECTOR('',#3215,0.999999999999999);
#1027=VECTOR('',#3234,0.999999999999999);
#1028=VECTOR('',#3237,0.999999999999999);
#1029=VECTOR('',#3256,0.999999999999999);
#1030=VECTOR('',#3259,0.999999999999999);
#1031=VECTOR('',#3278,0.999999999999999);
#1032=VECTOR('',#3281,0.999999999999999);
#1033=VECTOR('',#3300,0.999999999999999);
#1034=VECTOR('',#3303,0.999999999999999);
#1035=VECTOR('',#3322,0.999999999999999);
#1036=VECTOR('',#3325,0.999999999999999);
#1037=VECTOR('',#3344,0.999999999999999);
#1038=VECTOR('',#3347,0.999999999999999);
#1039=VECTOR('',#3366,0.999999999999999);
#1040=VECTOR('',#3369,0.999999999999999);
#1041=VECTOR('',#3388,0.999999999999999);
#1042=VECTOR('',#3391,0.999999999999999);
#1043=VECTOR('',#3410,0.999999999999999);
#1044=VECTOR('',#3413,0.999999999999999);
#1045=VECTOR('',#3432,0.999999999999999);
#1046=VECTOR('',#3435,0.999999999999999);
#1047=VECTOR('',#3474,2.15);
#1048=VECTOR('',#3479,2.15);
#1049=VECTOR('',#3484,2.15);
#1050=VECTOR('',#3489,2.15);
#1051=VECTOR('',#3492,1000.);
#1052=VECTOR('',#3493,1000.);
#1053=VECTOR('',#3494,1000.);
#1054=VECTOR('',#3495,1000.);
#1055=VECTOR('',#3498,1000.);
#1056=VECTOR('',#3499,1000.);
#1057=VECTOR('',#3500,1000.);
#1058=VECTOR('',#3501,1000.);
#1059=VECTOR('',#3504,1000.);
#1060=VECTOR('',#3505,1000.);
#1061=VECTOR('',#3506,1000.);
#1062=VECTOR('',#3507,1000.);
#1063=VECTOR('',#3508,1000.);
#1064=VECTOR('',#3509,1000.);
#1065=VECTOR('',#3510,1000.);
#1066=VECTOR('',#3511,1000.);
#1067=VECTOR('',#3514,1000.);
#1068=VECTOR('',#3515,1000.);
#1069=VECTOR('',#3516,1000.);
#1070=VECTOR('',#3517,1000.);
#1071=VECTOR('',#3518,1000.);
#1072=VECTOR('',#3521,1000.);
#1073=VECTOR('',#3522,1000.);
#1074=VECTOR('',#3523,1000.);
#1075=VECTOR('',#3524,1000.);
#1076=VECTOR('',#3525,1000.);
#1077=VECTOR('',#3528,1000.);
#1078=VECTOR('',#3529,1000.);
#1079=VECTOR('',#3530,1000.);
#1080=VECTOR('',#3533,1000.);
#1081=VECTOR('',#3534,1000.);
#1082=VECTOR('',#3537,1000.);
#1083=VECTOR('',#3538,1000.);
#1084=VECTOR('',#3541,1000.);
#1085=VECTOR('',#3548,1000.);
#1086=VECTOR('',#3553,1000.);
#1087=VECTOR('',#3560,1732.05080756886);
#1088=VECTOR('',#3585,1.61);
#1089=VECTOR('',#3590,2.);
#1090=VECTOR('',#3595,3.8);
#1091=VECTOR('',#3604,1000.);
#1092=VECTOR('',#3605,1000.);
#1093=VECTOR('',#3606,1000.);
#1094=VECTOR('',#3607,1000.);
#1095=VECTOR('',#3608,1000.);
#1096=VECTOR('',#3609,1000.);
#1097=VECTOR('',#3616,1000.);
#1098=VECTOR('',#3617,1000.);
#1099=VECTOR('',#3618,1000.);
#1100=VECTOR('',#3619,1000.);
#1101=VECTOR('',#3622,1000.);
#1102=VECTOR('',#3623,1000.);
#1103=VECTOR('',#3624,1000.);
#1104=VECTOR('',#3627,1000.);
#1105=VECTOR('',#3628,1000.);
#1106=VECTOR('',#3629,1000.);
#1107=VECTOR('',#3632,1000.);
#1108=VECTOR('',#3633,1000.);
#1109=VECTOR('',#3634,1000.);
#1110=VECTOR('',#3637,1000.);
#1111=VECTOR('',#3638,1000.);
#1112=VECTOR('',#3639,1000.);
#1113=VECTOR('',#3642,1000.);
#1114=VECTOR('',#3643,1000.);
#1115=VERTEX_POINT('',#3683);
#1116=VERTEX_POINT('',#3684);
#1117=VERTEX_POINT('',#3688);
#1118=VERTEX_POINT('',#3692);
#1119=VERTEX_POINT('',#3693);
#1120=VERTEX_POINT('',#3697);
#1121=VERTEX_POINT('',#3701);
#1122=VERTEX_POINT('',#3702);
#1123=VERTEX_POINT('',#3706);
#1124=VERTEX_POINT('',#3710);
#1125=VERTEX_POINT('',#3711);
#1126=VERTEX_POINT('',#3715);
#1127=VERTEX_POINT('',#3719);
#1128=VERTEX_POINT('',#3720);
#1129=VERTEX_POINT('',#3722);
#1130=VERTEX_POINT('',#3724);
#1131=VERTEX_POINT('',#3729);
#1132=VERTEX_POINT('',#3730);
#1133=VERTEX_POINT('',#3732);
#1134=VERTEX_POINT('',#3738);
#1135=VERTEX_POINT('',#3740);
#1136=VERTEX_POINT('',#3742);
#1137=VERTEX_POINT('',#3747);
#1138=VERTEX_POINT('',#3748);
#1139=VERTEX_POINT('',#3750);
#1140=VERTEX_POINT('',#3752);
#1141=VERTEX_POINT('',#3756);
#1142=VERTEX_POINT('',#3757);
#1143=VERTEX_POINT('',#3759);
#1144=VERTEX_POINT('',#3761);
#1145=VERTEX_POINT('',#3779);
#1146=VERTEX_POINT('',#3781);
#1147=VERTEX_POINT('',#3785);
#1148=VERTEX_POINT('',#3787);
#1149=VERTEX_POINT('',#3791);
#1150=VERTEX_POINT('',#3793);
#1151=VERTEX_POINT('',#3797);
#1152=VERTEX_POINT('',#3799);
#1153=VERTEX_POINT('',#3809);
#1154=VERTEX_POINT('',#3811);
#1155=VERTEX_POINT('',#3815);
#1156=VERTEX_POINT('',#3817);
#1157=VERTEX_POINT('',#5231);
#1158=VERTEX_POINT('',#5232);
#1159=VERTEX_POINT('',#5251);
#1160=VERTEX_POINT('',#5451);
#1161=VERTEX_POINT('',#5453);
#1162=VERTEX_POINT('',#5657);
#1163=VERTEX_POINT('',#7090);
#1164=VERTEX_POINT('',#7092);
#1165=VERTEX_POINT('',#7096);
#1166=VERTEX_POINT('',#7098);
#1167=VERTEX_POINT('',#7102);
#1168=VERTEX_POINT('',#7104);
#1169=VERTEX_POINT('',#7108);
#1170=VERTEX_POINT('',#7110);
#1171=VERTEX_POINT('',#7114);
#1172=VERTEX_POINT('',#7116);
#1173=VERTEX_POINT('',#7120);
#1174=VERTEX_POINT('',#7121);
#1175=VERTEX_POINT('',#7123);
#1176=VERTEX_POINT('',#7125);
#1177=VERTEX_POINT('',#7129);
#1178=VERTEX_POINT('',#7130);
#1179=VERTEX_POINT('',#7132);
#1180=VERTEX_POINT('',#7134);
#1181=VERTEX_POINT('',#7147);
#1182=VERTEX_POINT('',#7149);
#1183=VERTEX_POINT('',#7153);
#1184=VERTEX_POINT('',#7154);
#1185=VERTEX_POINT('',#7156);
#1186=VERTEX_POINT('',#7158);
#1187=VERTEX_POINT('',#7162);
#1188=VERTEX_POINT('',#7163);
#1189=VERTEX_POINT('',#7168);
#1190=VERTEX_POINT('',#7170);
#1191=VERTEX_POINT('',#7181);
#1192=VERTEX_POINT('',#7183);
#1193=VERTEX_POINT('',#7187);
#1194=VERTEX_POINT('',#7189);
#1195=VERTEX_POINT('',#7197);
#1196=VERTEX_POINT('',#7199);
#1197=VERTEX_POINT('',#7203);
#1198=VERTEX_POINT('',#7205);
#1199=VERTEX_POINT('',#7213);
#1200=VERTEX_POINT('',#7215);
#1201=VERTEX_POINT('',#7219);
#1202=VERTEX_POINT('',#7221);
#1203=VERTEX_POINT('',#7229);
#1204=VERTEX_POINT('',#7231);
#1205=VERTEX_POINT('',#7235);
#1206=VERTEX_POINT('',#7237);
#1207=VERTEX_POINT('',#7245);
#1208=VERTEX_POINT('',#7247);
#1209=VERTEX_POINT('',#7251);
#1210=VERTEX_POINT('',#7253);
#1211=VERTEX_POINT('',#7261);
#1212=VERTEX_POINT('',#7263);
#1213=VERTEX_POINT('',#7267);
#1214=VERTEX_POINT('',#7269);
#1215=VERTEX_POINT('',#7277);
#1216=VERTEX_POINT('',#7279);
#1217=VERTEX_POINT('',#7283);
#1218=VERTEX_POINT('',#7285);
#1219=VERTEX_POINT('',#7293);
#1220=VERTEX_POINT('',#7295);
#1221=VERTEX_POINT('',#7299);
#1222=VERTEX_POINT('',#7301);
#1223=VERTEX_POINT('',#7309);
#1224=VERTEX_POINT('',#7311);
#1225=VERTEX_POINT('',#7315);
#1226=VERTEX_POINT('',#7317);
#1227=VERTEX_POINT('',#7325);
#1228=VERTEX_POINT('',#7327);
#1229=VERTEX_POINT('',#7331);
#1230=VERTEX_POINT('',#7333);
#1231=VERTEX_POINT('',#7341);
#1232=VERTEX_POINT('',#7343);
#1233=VERTEX_POINT('',#7347);
#1234=VERTEX_POINT('',#7349);
#1235=VERTEX_POINT('',#7357);
#1236=VERTEX_POINT('',#7359);
#1237=VERTEX_POINT('',#7363);
#1238=VERTEX_POINT('',#7365);
#1239=VERTEX_POINT('',#7373);
#1240=VERTEX_POINT('',#7375);
#1241=VERTEX_POINT('',#7379);
#1242=VERTEX_POINT('',#7381);
#1243=VERTEX_POINT('',#7390);
#1244=VERTEX_POINT('',#7392);
#1245=VERTEX_POINT('',#7396);
#1246=VERTEX_POINT('',#7398);
#1247=VERTEX_POINT('',#7402);
#1248=VERTEX_POINT('',#7404);
#1249=VERTEX_POINT('',#7408);
#1250=VERTEX_POINT('',#7410);
#1251=VERTEX_POINT('',#7414);
#1252=VERTEX_POINT('',#7418);
#1253=VERTEX_POINT('',#7422);
#1254=VERTEX_POINT('',#7426);
#1255=VERTEX_POINT('',#7430);
#1256=VERTEX_POINT('',#7431);
#1257=VERTEX_POINT('',#7433);
#1258=VERTEX_POINT('',#7435);
#1259=VERTEX_POINT('',#7439);
#1260=VERTEX_POINT('',#7440);
#1261=VERTEX_POINT('',#7442);
#1262=VERTEX_POINT('',#7444);
#1263=VERTEX_POINT('',#7448);
#1264=VERTEX_POINT('',#7449);
#1265=VERTEX_POINT('',#7451);
#1266=VERTEX_POINT('',#7453);
#1267=VERTEX_POINT('',#7456);
#1268=VERTEX_POINT('',#7457);
#1269=VERTEX_POINT('',#7459);
#1270=VERTEX_POINT('',#7461);
#1271=VERTEX_POINT('',#7465);
#1272=VERTEX_POINT('',#7469);
#1273=VERTEX_POINT('',#7473);
#1274=VERTEX_POINT('',#7477);
#1275=VERTEX_POINT('',#7481);
#1276=VERTEX_POINT('',#7483);
#1277=VERTEX_POINT('',#7487);
#1278=VERTEX_POINT('',#7491);
#1279=VERTEX_POINT('',#7506);
#1280=VERTEX_POINT('',#7507);
#1281=VERTEX_POINT('',#7509);
#1282=VERTEX_POINT('',#7511);
#1283=VERTEX_POINT('',#7513);
#1284=VERTEX_POINT('',#7515);
#1285=VERTEX_POINT('',#7517);
#1286=VERTEX_POINT('',#7521);
#1287=VERTEX_POINT('',#7523);
#1288=VERTEX_POINT('',#7527);
#1289=VERTEX_POINT('',#7529);
#1290=VERTEX_POINT('',#7535);
#1291=VERTEX_POINT('',#7537);
#1292=VERTEX_POINT('',#7541);
#1293=VERTEX_POINT('',#7544);
#1294=VERTEX_POINT('',#7545);
#1295=VERTEX_POINT('',#7547);
#1296=VERTEX_POINT('',#7549);
#1297=VERTEX_POINT('',#7551);
#1298=VERTEX_POINT('',#7553);
#1299=VERTEX_POINT('',#7559);
#1300=VERTEX_POINT('',#7561);
#1301=VERTEX_POINT('',#7567);
#1302=VERTEX_POINT('',#7572);
#1303=VERTEX_POINT('',#7577);
#1304=VERTEX_POINT('',#7582);
#1305=EDGE_CURVE('',#1115,#1116,#803,.T.);
#1306=EDGE_CURVE('',#1116,#1116,#650,.T.);
#1307=EDGE_CURVE('',#1116,#1117,#804,.T.);
#1308=EDGE_CURVE('',#1117,#1117,#651,.T.);
#1309=EDGE_CURVE('',#1118,#1119,#805,.T.);
#1310=EDGE_CURVE('',#1119,#1119,#652,.T.);
#1311=EDGE_CURVE('',#1119,#1120,#806,.T.);
#1312=EDGE_CURVE('',#1120,#1120,#653,.T.);
#1313=EDGE_CURVE('',#1121,#1122,#807,.T.);
#1314=EDGE_CURVE('',#1122,#1122,#654,.T.);
#1315=EDGE_CURVE('',#1122,#1123,#808,.T.);
#1316=EDGE_CURVE('',#1123,#1123,#655,.T.);
#1317=EDGE_CURVE('',#1124,#1125,#809,.T.);
#1318=EDGE_CURVE('',#1125,#1125,#656,.T.);
#1319=EDGE_CURVE('',#1125,#1126,#810,.T.);
#1320=EDGE_CURVE('',#1126,#1126,#657,.T.);
#1321=EDGE_CURVE('',#1127,#1128,#252,.T.);
#1322=EDGE_CURVE('',#1129,#1127,#253,.T.);
#1323=EDGE_CURVE('',#1129,#1130,#811,.T.);
#1324=EDGE_CURVE('',#1130,#1130,#658,.T.);
#1325=EDGE_CURVE('',#1128,#1129,#254,.T.);
#1326=EDGE_CURVE('',#1131,#1132,#659,.T.);
#1327=EDGE_CURVE('',#1131,#1133,#812,.T.);
#1328=EDGE_CURVE('',#1133,#1133,#660,.T.);
#1329=EDGE_CURVE('',#1128,#1131,#813,.T.);
#1330=EDGE_CURVE('',#1132,#1127,#814,.T.);
#1331=EDGE_CURVE('',#1134,#1134,#661,.T.);
#1332=EDGE_CURVE('',#1134,#1135,#815,.T.);
#1333=EDGE_CURVE('',#1136,#1135,#662,.T.);
#1334=EDGE_CURVE('',#1127,#1136,#816,.T.);
#1335=EDGE_CURVE('',#1135,#1128,#817,.T.);
#1336=EDGE_CURVE('',#1137,#1138,#818,.T.);
#1337=EDGE_CURVE('',#1138,#1139,#819,.T.);
#1338=EDGE_CURVE('',#1139,#1140,#820,.T.);
#1339=EDGE_CURVE('',#1140,#1137,#821,.T.);
#1340=EDGE_CURVE('',#1141,#1142,#822,.T.);
#1341=EDGE_CURVE('',#1143,#1141,#823,.T.);
#1342=EDGE_CURVE('',#1144,#1143,#824,.T.);
#1343=EDGE_CURVE('',#1142,#1144,#825,.T.);
#1344=EDGE_CURVE('',#1138,#1142,#826,.T.);
#1345=EDGE_CURVE('',#1137,#1141,#827,.T.);
#1346=EDGE_CURVE('',#1139,#1144,#828,.T.);
#1347=EDGE_CURVE('',#1140,#1143,#829,.T.);
#1348=EDGE_CURVE('',#1132,#1131,#830,.T.);
#1349=EDGE_CURVE('',#1135,#1136,#831,.T.);
#1350=EDGE_CURVE('',#1145,#1145,#663,.T.);
#1351=EDGE_CURVE('',#1145,#1146,#832,.T.);
#1352=EDGE_CURVE('',#1146,#1146,#664,.T.);
#1353=EDGE_CURVE('',#1147,#1147,#665,.T.);
#1354=EDGE_CURVE('',#1147,#1148,#833,.T.);
#1355=EDGE_CURVE('',#1148,#1148,#666,.T.);
#1356=EDGE_CURVE('',#1149,#1149,#667,.T.);
#1357=EDGE_CURVE('',#1149,#1150,#834,.T.);
#1358=EDGE_CURVE('',#1150,#1150,#668,.T.);
#1359=EDGE_CURVE('',#1151,#1151,#669,.T.);
#1360=EDGE_CURVE('',#1151,#1152,#835,.T.);
#1361=EDGE_CURVE('',#1152,#1152,#670,.T.);
#1362=EDGE_CURVE('',#1153,#1153,#671,.T.);
#1363=EDGE_CURVE('',#1153,#1154,#836,.T.);
#1364=EDGE_CURVE('',#1154,#1154,#672,.T.);
#1365=EDGE_CURVE('',#1155,#1155,#673,.T.);
#1366=EDGE_CURVE('',#1155,#1156,#837,.T.);
#1367=EDGE_CURVE('',#1156,#1156,#674,.T.);
#1368=EDGE_CURVE('',#1157,#1158,#93,.T.);
#1369=EDGE_CURVE('',#1157,#1159,#91,.T.);
#1370=EDGE_CURVE('',#1159,#1160,#675,.T.);
#1371=EDGE_CURVE('',#1161,#1160,#92,.T.);
#1372=EDGE_CURVE('',#1161,#1158,#676,.T.);
#1373=EDGE_CURVE('',#1158,#1162,#838,.T.);
#1374=EDGE_CURVE('',#1162,#1161,#677,.T.);
#1375=EDGE_CURVE('',#1160,#1159,#678,.T.);
#1376=EDGE_CURVE('',#1162,#1157,#94,.T.);
#1377=EDGE_CURVE('',#1163,#1163,#679,.T.);
#1378=EDGE_CURVE('',#1163,#1164,#839,.T.);
#1379=EDGE_CURVE('',#1164,#1164,#680,.T.);
#1380=EDGE_CURVE('',#1165,#1165,#681,.T.);
#1381=EDGE_CURVE('',#1165,#1166,#840,.T.);
#1382=EDGE_CURVE('',#1166,#1166,#682,.T.);
#1383=EDGE_CURVE('',#1167,#1167,#683,.T.);
#1384=EDGE_CURVE('',#1167,#1168,#841,.T.);
#1385=EDGE_CURVE('',#1168,#1168,#684,.T.);
#1386=EDGE_CURVE('',#1169,#1169,#685,.T.);
#1387=EDGE_CURVE('',#1169,#1170,#842,.T.);
#1388=EDGE_CURVE('',#1170,#1170,#686,.T.);
#1389=EDGE_CURVE('',#1171,#1171,#687,.T.);
#1390=EDGE_CURVE('',#1171,#1172,#843,.T.);
#1391=EDGE_CURVE('',#1172,#1172,#688,.T.);
#1392=EDGE_CURVE('',#1173,#1174,#844,.T.);
#1393=EDGE_CURVE('',#1175,#1173,#845,.T.);
#1394=EDGE_CURVE('',#1176,#1175,#846,.T.);
#1395=EDGE_CURVE('',#1174,#1176,#847,.T.);
#1396=EDGE_CURVE('',#1177,#1178,#848,.T.);
#1397=EDGE_CURVE('',#1178,#1179,#849,.T.);
#1398=EDGE_CURVE('',#1179,#1180,#850,.T.);
#1399=EDGE_CURVE('',#1180,#1177,#851,.T.);
#1400=EDGE_CURVE('',#1178,#1174,#852,.T.);
#1401=EDGE_CURVE('',#1177,#1173,#853,.T.);
#1402=EDGE_CURVE('',#1179,#1176,#854,.T.);
#1403=EDGE_CURVE('',#1180,#1175,#855,.T.);
#1404=EDGE_CURVE('',#1181,#1181,#689,.T.);
#1405=EDGE_CURVE('',#1181,#1182,#856,.T.);
#1406=EDGE_CURVE('',#1182,#1182,#690,.T.);
#1407=EDGE_CURVE('',#1183,#1184,#691,.T.);
#1408=EDGE_CURVE('',#1183,#1185,#857,.T.);
#1409=EDGE_CURVE('',#1185,#1186,#692,.T.);
#1410=EDGE_CURVE('',#1184,#1186,#858,.T.);
#1411=EDGE_CURVE('',#1187,#1188,#693,.T.);
#1412=EDGE_CURVE('',#1186,#1187,#859,.T.);
#1413=EDGE_CURVE('',#1188,#1185,#860,.T.);
#1414=EDGE_CURVE('',#1189,#1188,#861,.T.);
#1415=EDGE_CURVE('',#1190,#1189,#694,.T.);
#1416=EDGE_CURVE('',#1190,#1187,#862,.T.);
#1417=EDGE_CURVE('',#1189,#1183,#863,.T.);
#1418=EDGE_CURVE('',#1184,#1190,#864,.T.);
#1419=EDGE_CURVE('',#1191,#1191,#695,.T.);
#1420=EDGE_CURVE('',#1191,#1192,#696,.T.);
#1421=EDGE_CURVE('',#1192,#1192,#697,.T.);
#1422=EDGE_CURVE('',#1193,#1193,#698,.T.);
#1423=EDGE_CURVE('',#1193,#1194,#699,.T.);
#1424=EDGE_CURVE('',#1194,#1194,#700,.T.);
#1425=EDGE_CURVE('',#1194,#1191,#865,.T.);
#1426=EDGE_CURVE('',#1192,#1193,#866,.T.);
#1427=EDGE_CURVE('',#1195,#1195,#701,.T.);
#1428=EDGE_CURVE('',#1195,#1196,#702,.T.);
#1429=EDGE_CURVE('',#1196,#1196,#703,.T.);
#1430=EDGE_CURVE('',#1197,#1197,#704,.T.);
#1431=EDGE_CURVE('',#1197,#1198,#705,.T.);
#1432=EDGE_CURVE('',#1198,#1198,#706,.T.);
#1433=EDGE_CURVE('',#1198,#1195,#867,.T.);
#1434=EDGE_CURVE('',#1196,#1197,#868,.T.);
#1435=EDGE_CURVE('',#1199,#1199,#707,.T.);
#1436=EDGE_CURVE('',#1199,#1200,#708,.T.);
#1437=EDGE_CURVE('',#1200,#1200,#709,.T.);
#1438=EDGE_CURVE('',#1201,#1201,#710,.T.);
#1439=EDGE_CURVE('',#1201,#1202,#711,.T.);
#1440=EDGE_CURVE('',#1202,#1202,#712,.T.);
#1441=EDGE_CURVE('',#1202,#1199,#869,.T.);
#1442=EDGE_CURVE('',#1200,#1201,#870,.T.);
#1443=EDGE_CURVE('',#1203,#1203,#713,.T.);
#1444=EDGE_CURVE('',#1203,#1204,#714,.T.);
#1445=EDGE_CURVE('',#1204,#1204,#715,.T.);
#1446=EDGE_CURVE('',#1205,#1205,#716,.T.);
#1447=EDGE_CURVE('',#1205,#1206,#717,.T.);
#1448=EDGE_CURVE('',#1206,#1206,#718,.T.);
#1449=EDGE_CURVE('',#1206,#1203,#871,.T.);
#1450=EDGE_CURVE('',#1204,#1205,#872,.T.);
#1451=EDGE_CURVE('',#1207,#1207,#719,.T.);
#1452=EDGE_CURVE('',#1207,#1208,#720,.T.);
#1453=EDGE_CURVE('',#1208,#1208,#721,.T.);
#1454=EDGE_CURVE('',#1209,#1209,#722,.T.);
#1455=EDGE_CURVE('',#1209,#1210,#723,.T.);
#1456=EDGE_CURVE('',#1210,#1210,#724,.T.);
#1457=EDGE_CURVE('',#1210,#1207,#873,.T.);
#1458=EDGE_CURVE('',#1208,#1209,#874,.T.);
#1459=EDGE_CURVE('',#1211,#1211,#725,.T.);
#1460=EDGE_CURVE('',#1211,#1212,#726,.T.);
#1461=EDGE_CURVE('',#1212,#1212,#727,.T.);
#1462=EDGE_CURVE('',#1213,#1213,#728,.T.);
#1463=EDGE_CURVE('',#1213,#1214,#729,.T.);
#1464=EDGE_CURVE('',#1214,#1214,#730,.T.);
#1465=EDGE_CURVE('',#1214,#1211,#875,.T.);
#1466=EDGE_CURVE('',#1212,#1213,#876,.T.);
#1467=EDGE_CURVE('',#1215,#1215,#731,.T.);
#1468=EDGE_CURVE('',#1215,#1216,#732,.T.);
#1469=EDGE_CURVE('',#1216,#1216,#733,.T.);
#1470=EDGE_CURVE('',#1217,#1217,#734,.T.);
#1471=EDGE_CURVE('',#1217,#1218,#735,.T.);
#1472=EDGE_CURVE('',#1218,#1218,#736,.T.);
#1473=EDGE_CURVE('',#1218,#1215,#877,.T.);
#1474=EDGE_CURVE('',#1216,#1217,#878,.T.);
#1475=EDGE_CURVE('',#1219,#1219,#737,.T.);
#1476=EDGE_CURVE('',#1219,#1220,#738,.T.);
#1477=EDGE_CURVE('',#1220,#1220,#739,.T.);
#1478=EDGE_CURVE('',#1221,#1221,#740,.T.);
#1479=EDGE_CURVE('',#1221,#1222,#741,.T.);
#1480=EDGE_CURVE('',#1222,#1222,#742,.T.);
#1481=EDGE_CURVE('',#1222,#1219,#879,.T.);
#1482=EDGE_CURVE('',#1220,#1221,#880,.T.);
#1483=EDGE_CURVE('',#1223,#1223,#743,.T.);
#1484=EDGE_CURVE('',#1223,#1224,#744,.T.);
#1485=EDGE_CURVE('',#1224,#1224,#745,.T.);
#1486=EDGE_CURVE('',#1225,#1225,#746,.T.);
#1487=EDGE_CURVE('',#1225,#1226,#747,.T.);
#1488=EDGE_CURVE('',#1226,#1226,#748,.T.);
#1489=EDGE_CURVE('',#1226,#1223,#881,.T.);
#1490=EDGE_CURVE('',#1224,#1225,#882,.T.);
#1491=EDGE_CURVE('',#1227,#1227,#749,.T.);
#1492=EDGE_CURVE('',#1227,#1228,#750,.T.);
#1493=EDGE_CURVE('',#1228,#1228,#751,.T.);
#1494=EDGE_CURVE('',#1229,#1229,#752,.T.);
#1495=EDGE_CURVE('',#1229,#1230,#753,.T.);
#1496=EDGE_CURVE('',#1230,#1230,#754,.T.);
#1497=EDGE_CURVE('',#1230,#1227,#883,.T.);
#1498=EDGE_CURVE('',#1228,#1229,#884,.T.);
#1499=EDGE_CURVE('',#1231,#1231,#755,.T.);
#1500=EDGE_CURVE('',#1231,#1232,#756,.T.);
#1501=EDGE_CURVE('',#1232,#1232,#757,.T.);
#1502=EDGE_CURVE('',#1233,#1233,#758,.T.);
#1503=EDGE_CURVE('',#1233,#1234,#759,.T.);
#1504=EDGE_CURVE('',#1234,#1234,#760,.T.);
#1505=EDGE_CURVE('',#1234,#1231,#885,.T.);
#1506=EDGE_CURVE('',#1232,#1233,#886,.T.);
#1507=EDGE_CURVE('',#1235,#1235,#761,.T.);
#1508=EDGE_CURVE('',#1235,#1236,#762,.T.);
#1509=EDGE_CURVE('',#1236,#1236,#763,.T.);
#1510=EDGE_CURVE('',#1237,#1237,#764,.T.);
#1511=EDGE_CURVE('',#1237,#1238,#765,.T.);
#1512=EDGE_CURVE('',#1238,#1238,#766,.T.);
#1513=EDGE_CURVE('',#1238,#1235,#887,.T.);
#1514=EDGE_CURVE('',#1236,#1237,#888,.T.);
#1515=EDGE_CURVE('',#1239,#1239,#767,.T.);
#1516=EDGE_CURVE('',#1239,#1240,#768,.T.);
#1517=EDGE_CURVE('',#1240,#1240,#769,.T.);
#1518=EDGE_CURVE('',#1241,#1241,#770,.T.);
#1519=EDGE_CURVE('',#1241,#1242,#771,.T.);
#1520=EDGE_CURVE('',#1242,#1242,#772,.T.);
#1521=EDGE_CURVE('',#1242,#1239,#889,.T.);
#1522=EDGE_CURVE('',#1240,#1241,#890,.T.);
#1523=EDGE_CURVE('',#1243,#1243,#773,.T.);
#1524=EDGE_CURVE('',#1243,#1244,#774,.T.);
#1525=EDGE_CURVE('',#1244,#1244,#775,.T.);
#1526=EDGE_CURVE('',#1245,#1245,#776,.T.);
#1527=EDGE_CURVE('',#1245,#1246,#777,.T.);
#1528=EDGE_CURVE('',#1246,#1246,#778,.T.);
#1529=EDGE_CURVE('',#1247,#1247,#779,.T.);
#1530=EDGE_CURVE('',#1247,#1248,#780,.T.);
#1531=EDGE_CURVE('',#1248,#1248,#781,.T.);
#1532=EDGE_CURVE('',#1249,#1249,#782,.T.);
#1533=EDGE_CURVE('',#1249,#1250,#783,.T.);
#1534=EDGE_CURVE('',#1250,#1250,#784,.T.);
#1535=EDGE_CURVE('',#1251,#1251,#785,.T.);
#1536=EDGE_CURVE('',#1251,#1249,#891,.T.);
#1537=EDGE_CURVE('',#1252,#1252,#786,.T.);
#1538=EDGE_CURVE('',#1252,#1247,#892,.T.);
#1539=EDGE_CURVE('',#1253,#1253,#787,.T.);
#1540=EDGE_CURVE('',#1253,#1245,#893,.T.);
#1541=EDGE_CURVE('',#1254,#1254,#788,.T.);
#1542=EDGE_CURVE('',#1254,#1243,#894,.T.);
#1543=EDGE_CURVE('',#1255,#1256,#895,.T.);
#1544=EDGE_CURVE('',#1257,#1255,#896,.T.);
#1545=EDGE_CURVE('',#1258,#1257,#897,.T.);
#1546=EDGE_CURVE('',#1258,#1256,#898,.T.);
#1547=EDGE_CURVE('',#1259,#1260,#899,.T.);
#1548=EDGE_CURVE('',#1261,#1259,#900,.T.);
#1549=EDGE_CURVE('',#1262,#1261,#901,.T.);
#1550=EDGE_CURVE('',#1262,#1260,#902,.T.);
#1551=EDGE_CURVE('',#1263,#1264,#903,.T.);
#1552=EDGE_CURVE('',#1265,#1263,#904,.T.);
#1553=EDGE_CURVE('',#1266,#1265,#905,.T.);
#1554=EDGE_CURVE('',#1264,#1266,#906,.T.);
#1555=EDGE_CURVE('',#1267,#1268,#907,.T.);
#1556=EDGE_CURVE('',#1268,#1269,#908,.T.);
#1557=EDGE_CURVE('',#1269,#1270,#909,.T.);
#1558=EDGE_CURVE('',#1270,#1267,#910,.T.);
#1559=EDGE_CURVE('',#1271,#1264,#911,.T.);
#1560=EDGE_CURVE('',#1256,#1271,#912,.T.);
#1561=EDGE_CURVE('',#1261,#1258,#913,.T.);
#1562=EDGE_CURVE('',#1272,#1259,#914,.T.);
#1563=EDGE_CURVE('',#1272,#1263,#915,.T.);
#1564=EDGE_CURVE('',#1273,#1265,#916,.T.);
#1565=EDGE_CURVE('',#1260,#1273,#917,.T.);
#1566=EDGE_CURVE('',#1257,#1262,#918,.T.);
#1567=EDGE_CURVE('',#1274,#1255,#919,.T.);
#1568=EDGE_CURVE('',#1274,#1266,#920,.T.);
#1569=EDGE_CURVE('',#1275,#1267,#921,.T.);
#1570=EDGE_CURVE('',#1275,#1276,#922,.T.);
#1571=EDGE_CURVE('',#1276,#1268,#923,.T.);
#1572=EDGE_CURVE('',#1276,#1277,#924,.T.);
#1573=EDGE_CURVE('',#1277,#1269,#925,.T.);
#1574=EDGE_CURVE('',#1277,#1278,#926,.T.);
#1575=EDGE_CURVE('',#1278,#1270,#927,.T.);
#1576=EDGE_CURVE('',#1278,#1275,#928,.T.);
#1577=EDGE_CURVE('',#1273,#1272,#929,.T.);
#1578=EDGE_CURVE('',#1271,#1274,#930,.T.);
#1579=EDGE_CURVE('',#1279,#1280,#931,.T.);
#1580=EDGE_CURVE('',#1280,#1281,#789,.T.);
#1581=EDGE_CURVE('',#1281,#1282,#790,.T.);
#1582=EDGE_CURVE('',#1282,#1283,#791,.T.);
#1583=EDGE_CURVE('',#1283,#1284,#792,.T.);
#1584=EDGE_CURVE('',#1284,#1285,#793,.T.);
#1585=EDGE_CURVE('',#1285,#1280,#794,.T.);
#1586=EDGE_CURVE('',#1286,#1286,#795,.T.);
#1587=EDGE_CURVE('',#1286,#1287,#796,.T.);
#1588=EDGE_CURVE('',#1287,#1287,#797,.T.);
#1589=EDGE_CURVE('',#1288,#1288,#798,.T.);
#1590=EDGE_CURVE('',#1288,#1289,#932,.T.);
#1591=EDGE_CURVE('',#1289,#1289,#799,.T.);
#1592=EDGE_CURVE('',#1287,#1288,#933,.T.);
#1593=EDGE_CURVE('',#1290,#1290,#800,.T.);
#1594=EDGE_CURVE('',#1290,#1291,#934,.T.);
#1595=EDGE_CURVE('',#1291,#1291,#801,.T.);
#1596=EDGE_CURVE('',#1292,#1292,#802,.T.);
#1597=EDGE_CURVE('',#1293,#1294,#935,.T.);
#1598=EDGE_CURVE('',#1294,#1295,#936,.T.);
#1599=EDGE_CURVE('',#1295,#1296,#937,.T.);
#1600=EDGE_CURVE('',#1296,#1297,#938,.T.);
#1601=EDGE_CURVE('',#1297,#1298,#939,.T.);
#1602=EDGE_CURVE('',#1298,#1293,#940,.T.);
#1603=EDGE_CURVE('',#1299,#1282,#941,.T.);
#1604=EDGE_CURVE('',#1282,#1300,#942,.T.);
#1605=EDGE_CURVE('',#1300,#1295,#943,.T.);
#1606=EDGE_CURVE('',#1299,#1294,#944,.T.);
#1607=EDGE_CURVE('',#1300,#1281,#945,.T.);
#1608=EDGE_CURVE('',#1281,#1301,#946,.T.);
#1609=EDGE_CURVE('',#1301,#1296,#947,.T.);
#1610=EDGE_CURVE('',#1301,#1280,#948,.T.);
#1611=EDGE_CURVE('',#1280,#1302,#949,.T.);
#1612=EDGE_CURVE('',#1302,#1297,#950,.T.);
#1613=EDGE_CURVE('',#1302,#1285,#951,.T.);
#1614=EDGE_CURVE('',#1285,#1303,#952,.T.);
#1615=EDGE_CURVE('',#1303,#1298,#953,.T.);
#1616=EDGE_CURVE('',#1303,#1284,#954,.T.);
#1617=EDGE_CURVE('',#1284,#1304,#955,.T.);
#1618=EDGE_CURVE('',#1304,#1293,#956,.T.);
#1619=EDGE_CURVE('',#1304,#1283,#957,.T.);
#1620=EDGE_CURVE('',#1283,#1299,#958,.T.);
#1621=ORIENTED_EDGE('',*,*,#1305,.T.);
#1622=ORIENTED_EDGE('',*,*,#1306,.T.);
#1623=ORIENTED_EDGE('',*,*,#1305,.F.);
#1624=ORIENTED_EDGE('',*,*,#1306,.F.);
#1625=ORIENTED_EDGE('',*,*,#1307,.T.);
#1626=ORIENTED_EDGE('',*,*,#1308,.T.);
#1627=ORIENTED_EDGE('',*,*,#1307,.F.);
#1628=ORIENTED_EDGE('',*,*,#1309,.T.);
#1629=ORIENTED_EDGE('',*,*,#1310,.T.);
#1630=ORIENTED_EDGE('',*,*,#1309,.F.);
#1631=ORIENTED_EDGE('',*,*,#1310,.F.);
#1632=ORIENTED_EDGE('',*,*,#1311,.T.);
#1633=ORIENTED_EDGE('',*,*,#1312,.T.);
#1634=ORIENTED_EDGE('',*,*,#1311,.F.);
#1635=ORIENTED_EDGE('',*,*,#1313,.T.);
#1636=ORIENTED_EDGE('',*,*,#1314,.T.);
#1637=ORIENTED_EDGE('',*,*,#1313,.F.);
#1638=ORIENTED_EDGE('',*,*,#1314,.F.);
#1639=ORIENTED_EDGE('',*,*,#1315,.T.);
#1640=ORIENTED_EDGE('',*,*,#1316,.T.);
#1641=ORIENTED_EDGE('',*,*,#1315,.F.);
#1642=ORIENTED_EDGE('',*,*,#1317,.T.);
#1643=ORIENTED_EDGE('',*,*,#1318,.T.);
#1644=ORIENTED_EDGE('',*,*,#1317,.F.);
#1645=ORIENTED_EDGE('',*,*,#1318,.F.);
#1646=ORIENTED_EDGE('',*,*,#1319,.T.);
#1647=ORIENTED_EDGE('',*,*,#1320,.T.);
#1648=ORIENTED_EDGE('',*,*,#1319,.F.);
#1649=ORIENTED_EDGE('',*,*,#1321,.F.);
#1650=ORIENTED_EDGE('',*,*,#1322,.F.);
#1651=ORIENTED_EDGE('',*,*,#1323,.T.);
#1652=ORIENTED_EDGE('',*,*,#1324,.T.);
#1653=ORIENTED_EDGE('',*,*,#1323,.F.);
#1654=ORIENTED_EDGE('',*,*,#1325,.F.);
#1655=ORIENTED_EDGE('',*,*,#1326,.F.);
#1656=ORIENTED_EDGE('',*,*,#1327,.T.);
#1657=ORIENTED_EDGE('',*,*,#1328,.F.);
#1658=ORIENTED_EDGE('',*,*,#1327,.F.);
#1659=ORIENTED_EDGE('',*,*,#1329,.F.);
#1660=ORIENTED_EDGE('',*,*,#1325,.T.);
#1661=ORIENTED_EDGE('',*,*,#1322,.T.);
#1662=ORIENTED_EDGE('',*,*,#1330,.F.);
#1663=ORIENTED_EDGE('',*,*,#1331,.T.);
#1664=ORIENTED_EDGE('',*,*,#1332,.T.);
#1665=ORIENTED_EDGE('',*,*,#1333,.F.);
#1666=ORIENTED_EDGE('',*,*,#1334,.F.);
#1667=ORIENTED_EDGE('',*,*,#1321,.T.);
#1668=ORIENTED_EDGE('',*,*,#1335,.F.);
#1669=ORIENTED_EDGE('',*,*,#1332,.F.);
#1670=ORIENTED_EDGE('',*,*,#1336,.T.);
#1671=ORIENTED_EDGE('',*,*,#1337,.T.);
#1672=ORIENTED_EDGE('',*,*,#1338,.T.);
#1673=ORIENTED_EDGE('',*,*,#1339,.T.);
#1674=ORIENTED_EDGE('',*,*,#1331,.F.);
#1675=ORIENTED_EDGE('',*,*,#1340,.F.);
#1676=ORIENTED_EDGE('',*,*,#1341,.F.);
#1677=ORIENTED_EDGE('',*,*,#1342,.F.);
#1678=ORIENTED_EDGE('',*,*,#1343,.F.);
#1679=ORIENTED_EDGE('',*,*,#1328,.T.);
#1680=ORIENTED_EDGE('',*,*,#1340,.T.);
#1681=ORIENTED_EDGE('',*,*,#1344,.F.);
#1682=ORIENTED_EDGE('',*,*,#1336,.F.);
#1683=ORIENTED_EDGE('',*,*,#1345,.T.);
#1684=ORIENTED_EDGE('',*,*,#1343,.T.);
#1685=ORIENTED_EDGE('',*,*,#1346,.F.);
#1686=ORIENTED_EDGE('',*,*,#1337,.F.);
#1687=ORIENTED_EDGE('',*,*,#1344,.T.);
#1688=ORIENTED_EDGE('',*,*,#1308,.F.);
#1689=ORIENTED_EDGE('',*,*,#1312,.F.);
#1690=ORIENTED_EDGE('',*,*,#1316,.F.);
#1691=ORIENTED_EDGE('',*,*,#1320,.F.);
#1692=ORIENTED_EDGE('',*,*,#1324,.F.);
#1693=ORIENTED_EDGE('',*,*,#1342,.T.);
#1694=ORIENTED_EDGE('',*,*,#1347,.F.);
#1695=ORIENTED_EDGE('',*,*,#1338,.F.);
#1696=ORIENTED_EDGE('',*,*,#1346,.T.);
#1697=ORIENTED_EDGE('',*,*,#1341,.T.);
#1698=ORIENTED_EDGE('',*,*,#1345,.F.);
#1699=ORIENTED_EDGE('',*,*,#1339,.F.);
#1700=ORIENTED_EDGE('',*,*,#1347,.T.);
#1701=ORIENTED_EDGE('',*,*,#1348,.T.);
#1702=ORIENTED_EDGE('',*,*,#1326,.T.);
#1703=ORIENTED_EDGE('',*,*,#1349,.T.);
#1704=ORIENTED_EDGE('',*,*,#1333,.T.);
#1705=ORIENTED_EDGE('',*,*,#1349,.F.);
#1706=ORIENTED_EDGE('',*,*,#1335,.T.);
#1707=ORIENTED_EDGE('',*,*,#1329,.T.);
#1708=ORIENTED_EDGE('',*,*,#1348,.F.);
#1709=ORIENTED_EDGE('',*,*,#1330,.T.);
#1710=ORIENTED_EDGE('',*,*,#1334,.T.);
#1711=ORIENTED_EDGE('',*,*,#1350,.F.);
#1712=ORIENTED_EDGE('',*,*,#1351,.T.);
#1713=ORIENTED_EDGE('',*,*,#1352,.T.);
#1714=ORIENTED_EDGE('',*,*,#1351,.F.);
#1715=ORIENTED_EDGE('',*,*,#1353,.F.);
#1716=ORIENTED_EDGE('',*,*,#1354,.T.);
#1717=ORIENTED_EDGE('',*,*,#1355,.T.);
#1718=ORIENTED_EDGE('',*,*,#1354,.F.);
#1719=ORIENTED_EDGE('',*,*,#1356,.F.);
#1720=ORIENTED_EDGE('',*,*,#1357,.T.);
#1721=ORIENTED_EDGE('',*,*,#1358,.T.);
#1722=ORIENTED_EDGE('',*,*,#1357,.F.);
#1723=ORIENTED_EDGE('',*,*,#1359,.F.);
#1724=ORIENTED_EDGE('',*,*,#1360,.T.);
#1725=ORIENTED_EDGE('',*,*,#1361,.F.);
#1726=ORIENTED_EDGE('',*,*,#1360,.F.);
#1727=ORIENTED_EDGE('',*,*,#1359,.T.);
#1728=ORIENTED_EDGE('',*,*,#1358,.F.);
#1729=ORIENTED_EDGE('',*,*,#1356,.T.);
#1730=ORIENTED_EDGE('',*,*,#1355,.F.);
#1731=ORIENTED_EDGE('',*,*,#1361,.T.);
#1732=ORIENTED_EDGE('',*,*,#1353,.T.);
#1733=ORIENTED_EDGE('',*,*,#1352,.F.);
#1734=ORIENTED_EDGE('',*,*,#1350,.T.);
#1735=ORIENTED_EDGE('',*,*,#1362,.T.);
#1736=ORIENTED_EDGE('',*,*,#1363,.T.);
#1737=ORIENTED_EDGE('',*,*,#1364,.F.);
#1738=ORIENTED_EDGE('',*,*,#1363,.F.);
#1739=ORIENTED_EDGE('',*,*,#1365,.T.);
#1740=ORIENTED_EDGE('',*,*,#1366,.T.);
#1741=ORIENTED_EDGE('',*,*,#1367,.F.);
#1742=ORIENTED_EDGE('',*,*,#1366,.F.);
#1743=ORIENTED_EDGE('',*,*,#1365,.F.);
#1744=ORIENTED_EDGE('',*,*,#1364,.T.);
#1745=ORIENTED_EDGE('',*,*,#1362,.F.);
#1746=ORIENTED_EDGE('',*,*,#1367,.T.);
#1747=ORIENTED_EDGE('',*,*,#1368,.F.);
#1748=ORIENTED_EDGE('',*,*,#1369,.T.);
#1749=ORIENTED_EDGE('',*,*,#1370,.T.);
#1750=ORIENTED_EDGE('',*,*,#1371,.F.);
#1751=ORIENTED_EDGE('',*,*,#1372,.T.);
#1752=ORIENTED_EDGE('',*,*,#1373,.F.);
#1753=ORIENTED_EDGE('',*,*,#1372,.F.);
#1754=ORIENTED_EDGE('',*,*,#1374,.F.);
#1755=ORIENTED_EDGE('',*,*,#1375,.F.);
#1756=ORIENTED_EDGE('',*,*,#1370,.F.);
#1757=ORIENTED_EDGE('',*,*,#1369,.F.);
#1758=ORIENTED_EDGE('',*,*,#1376,.F.);
#1759=ORIENTED_EDGE('',*,*,#1374,.T.);
#1760=ORIENTED_EDGE('',*,*,#1371,.T.);
#1761=ORIENTED_EDGE('',*,*,#1375,.T.);
#1762=ORIENTED_EDGE('',*,*,#1373,.T.);
#1763=ORIENTED_EDGE('',*,*,#1376,.T.);
#1764=ORIENTED_EDGE('',*,*,#1368,.T.);
#1765=ORIENTED_EDGE('',*,*,#1377,.F.);
#1766=ORIENTED_EDGE('',*,*,#1378,.T.);
#1767=ORIENTED_EDGE('',*,*,#1379,.F.);
#1768=ORIENTED_EDGE('',*,*,#1378,.F.);
#1769=ORIENTED_EDGE('',*,*,#1380,.F.);
#1770=ORIENTED_EDGE('',*,*,#1381,.T.);
#1771=ORIENTED_EDGE('',*,*,#1382,.F.);
#1772=ORIENTED_EDGE('',*,*,#1381,.F.);
#1773=ORIENTED_EDGE('',*,*,#1383,.F.);
#1774=ORIENTED_EDGE('',*,*,#1384,.T.);
#1775=ORIENTED_EDGE('',*,*,#1385,.F.);
#1776=ORIENTED_EDGE('',*,*,#1384,.F.);
#1777=ORIENTED_EDGE('',*,*,#1386,.F.);
#1778=ORIENTED_EDGE('',*,*,#1387,.T.);
#1779=ORIENTED_EDGE('',*,*,#1388,.F.);
#1780=ORIENTED_EDGE('',*,*,#1387,.F.);
#1781=ORIENTED_EDGE('',*,*,#1389,.T.);
#1782=ORIENTED_EDGE('',*,*,#1390,.T.);
#1783=ORIENTED_EDGE('',*,*,#1391,.F.);
#1784=ORIENTED_EDGE('',*,*,#1390,.F.);
#1785=ORIENTED_EDGE('',*,*,#1392,.F.);
#1786=ORIENTED_EDGE('',*,*,#1393,.F.);
#1787=ORIENTED_EDGE('',*,*,#1394,.F.);
#1788=ORIENTED_EDGE('',*,*,#1395,.F.);
#1789=ORIENTED_EDGE('',*,*,#1386,.T.);
#1790=ORIENTED_EDGE('',*,*,#1383,.T.);
#1791=ORIENTED_EDGE('',*,*,#1377,.T.);
#1792=ORIENTED_EDGE('',*,*,#1380,.T.);
#1793=ORIENTED_EDGE('',*,*,#1391,.T.);
#1794=ORIENTED_EDGE('',*,*,#1396,.T.);
#1795=ORIENTED_EDGE('',*,*,#1397,.T.);
#1796=ORIENTED_EDGE('',*,*,#1398,.T.);
#1797=ORIENTED_EDGE('',*,*,#1399,.T.);
#1798=ORIENTED_EDGE('',*,*,#1389,.F.);
#1799=ORIENTED_EDGE('',*,*,#1379,.T.);
#1800=ORIENTED_EDGE('',*,*,#1382,.T.);
#1801=ORIENTED_EDGE('',*,*,#1385,.T.);
#1802=ORIENTED_EDGE('',*,*,#1388,.T.);
#1803=ORIENTED_EDGE('',*,*,#1392,.T.);
#1804=ORIENTED_EDGE('',*,*,#1400,.F.);
#1805=ORIENTED_EDGE('',*,*,#1396,.F.);
#1806=ORIENTED_EDGE('',*,*,#1401,.T.);
#1807=ORIENTED_EDGE('',*,*,#1395,.T.);
#1808=ORIENTED_EDGE('',*,*,#1402,.F.);
#1809=ORIENTED_EDGE('',*,*,#1397,.F.);
#1810=ORIENTED_EDGE('',*,*,#1400,.T.);
#1811=ORIENTED_EDGE('',*,*,#1394,.T.);
#1812=ORIENTED_EDGE('',*,*,#1403,.F.);
#1813=ORIENTED_EDGE('',*,*,#1398,.F.);
#1814=ORIENTED_EDGE('',*,*,#1402,.T.);
#1815=ORIENTED_EDGE('',*,*,#1393,.T.);
#1816=ORIENTED_EDGE('',*,*,#1401,.F.);
#1817=ORIENTED_EDGE('',*,*,#1399,.F.);
#1818=ORIENTED_EDGE('',*,*,#1403,.T.);
#1819=ORIENTED_EDGE('',*,*,#1404,.T.);
#1820=ORIENTED_EDGE('',*,*,#1405,.T.);
#1821=ORIENTED_EDGE('',*,*,#1406,.F.);
#1822=ORIENTED_EDGE('',*,*,#1405,.F.);
#1823=ORIENTED_EDGE('',*,*,#1407,.F.);
#1824=ORIENTED_EDGE('',*,*,#1408,.T.);
#1825=ORIENTED_EDGE('',*,*,#1409,.T.);
#1826=ORIENTED_EDGE('',*,*,#1410,.F.);
#1827=ORIENTED_EDGE('',*,*,#1411,.F.);
#1828=ORIENTED_EDGE('',*,*,#1412,.F.);
#1829=ORIENTED_EDGE('',*,*,#1409,.F.);
#1830=ORIENTED_EDGE('',*,*,#1413,.F.);
#1831=ORIENTED_EDGE('',*,*,#1406,.T.);
#1832=ORIENTED_EDGE('',*,*,#1411,.T.);
#1833=ORIENTED_EDGE('',*,*,#1414,.F.);
#1834=ORIENTED_EDGE('',*,*,#1415,.F.);
#1835=ORIENTED_EDGE('',*,*,#1416,.T.);
#1836=ORIENTED_EDGE('',*,*,#1413,.T.);
#1837=ORIENTED_EDGE('',*,*,#1408,.F.);
#1838=ORIENTED_EDGE('',*,*,#1417,.F.);
#1839=ORIENTED_EDGE('',*,*,#1414,.T.);
#1840=ORIENTED_EDGE('',*,*,#1412,.T.);
#1841=ORIENTED_EDGE('',*,*,#1416,.F.);
#1842=ORIENTED_EDGE('',*,*,#1418,.F.);
#1843=ORIENTED_EDGE('',*,*,#1410,.T.);
#1844=ORIENTED_EDGE('',*,*,#1404,.F.);
#1845=ORIENTED_EDGE('',*,*,#1415,.T.);
#1846=ORIENTED_EDGE('',*,*,#1417,.T.);
#1847=ORIENTED_EDGE('',*,*,#1407,.T.);
#1848=ORIENTED_EDGE('',*,*,#1418,.T.);
#1849=ORIENTED_EDGE('',*,*,#1419,.T.);
#1850=ORIENTED_EDGE('',*,*,#1420,.T.);
#1851=ORIENTED_EDGE('',*,*,#1421,.F.);
#1852=ORIENTED_EDGE('',*,*,#1420,.F.);
#1853=ORIENTED_EDGE('',*,*,#1422,.T.);
#1854=ORIENTED_EDGE('',*,*,#1423,.T.);
#1855=ORIENTED_EDGE('',*,*,#1424,.F.);
#1856=ORIENTED_EDGE('',*,*,#1423,.F.);
#1857=ORIENTED_EDGE('',*,*,#1424,.T.);
#1858=ORIENTED_EDGE('',*,*,#1425,.T.);
#1859=ORIENTED_EDGE('',*,*,#1419,.F.);
#1860=ORIENTED_EDGE('',*,*,#1425,.F.);
#1861=ORIENTED_EDGE('',*,*,#1421,.T.);
#1862=ORIENTED_EDGE('',*,*,#1426,.T.);
#1863=ORIENTED_EDGE('',*,*,#1422,.F.);
#1864=ORIENTED_EDGE('',*,*,#1426,.F.);
#1865=ORIENTED_EDGE('',*,*,#1427,.T.);
#1866=ORIENTED_EDGE('',*,*,#1428,.T.);
#1867=ORIENTED_EDGE('',*,*,#1429,.F.);
#1868=ORIENTED_EDGE('',*,*,#1428,.F.);
#1869=ORIENTED_EDGE('',*,*,#1430,.T.);
#1870=ORIENTED_EDGE('',*,*,#1431,.T.);
#1871=ORIENTED_EDGE('',*,*,#1432,.F.);
#1872=ORIENTED_EDGE('',*,*,#1431,.F.);
#1873=ORIENTED_EDGE('',*,*,#1432,.T.);
#1874=ORIENTED_EDGE('',*,*,#1433,.T.);
#1875=ORIENTED_EDGE('',*,*,#1427,.F.);
#1876=ORIENTED_EDGE('',*,*,#1433,.F.);
#1877=ORIENTED_EDGE('',*,*,#1429,.T.);
#1878=ORIENTED_EDGE('',*,*,#1434,.T.);
#1879=ORIENTED_EDGE('',*,*,#1430,.F.);
#1880=ORIENTED_EDGE('',*,*,#1434,.F.);
#1881=ORIENTED_EDGE('',*,*,#1435,.T.);
#1882=ORIENTED_EDGE('',*,*,#1436,.T.);
#1883=ORIENTED_EDGE('',*,*,#1437,.F.);
#1884=ORIENTED_EDGE('',*,*,#1436,.F.);
#1885=ORIENTED_EDGE('',*,*,#1438,.T.);
#1886=ORIENTED_EDGE('',*,*,#1439,.T.);
#1887=ORIENTED_EDGE('',*,*,#1440,.F.);
#1888=ORIENTED_EDGE('',*,*,#1439,.F.);
#1889=ORIENTED_EDGE('',*,*,#1440,.T.);
#1890=ORIENTED_EDGE('',*,*,#1441,.T.);
#1891=ORIENTED_EDGE('',*,*,#1435,.F.);
#1892=ORIENTED_EDGE('',*,*,#1441,.F.);
#1893=ORIENTED_EDGE('',*,*,#1437,.T.);
#1894=ORIENTED_EDGE('',*,*,#1442,.T.);
#1895=ORIENTED_EDGE('',*,*,#1438,.F.);
#1896=ORIENTED_EDGE('',*,*,#1442,.F.);
#1897=ORIENTED_EDGE('',*,*,#1443,.T.);
#1898=ORIENTED_EDGE('',*,*,#1444,.T.);
#1899=ORIENTED_EDGE('',*,*,#1445,.F.);
#1900=ORIENTED_EDGE('',*,*,#1444,.F.);
#1901=ORIENTED_EDGE('',*,*,#1446,.T.);
#1902=ORIENTED_EDGE('',*,*,#1447,.T.);
#1903=ORIENTED_EDGE('',*,*,#1448,.F.);
#1904=ORIENTED_EDGE('',*,*,#1447,.F.);
#1905=ORIENTED_EDGE('',*,*,#1448,.T.);
#1906=ORIENTED_EDGE('',*,*,#1449,.T.);
#1907=ORIENTED_EDGE('',*,*,#1443,.F.);
#1908=ORIENTED_EDGE('',*,*,#1449,.F.);
#1909=ORIENTED_EDGE('',*,*,#1445,.T.);
#1910=ORIENTED_EDGE('',*,*,#1450,.T.);
#1911=ORIENTED_EDGE('',*,*,#1446,.F.);
#1912=ORIENTED_EDGE('',*,*,#1450,.F.);
#1913=ORIENTED_EDGE('',*,*,#1451,.T.);
#1914=ORIENTED_EDGE('',*,*,#1452,.T.);
#1915=ORIENTED_EDGE('',*,*,#1453,.F.);
#1916=ORIENTED_EDGE('',*,*,#1452,.F.);
#1917=ORIENTED_EDGE('',*,*,#1454,.T.);
#1918=ORIENTED_EDGE('',*,*,#1455,.T.);
#1919=ORIENTED_EDGE('',*,*,#1456,.F.);
#1920=ORIENTED_EDGE('',*,*,#1455,.F.);
#1921=ORIENTED_EDGE('',*,*,#1456,.T.);
#1922=ORIENTED_EDGE('',*,*,#1457,.T.);
#1923=ORIENTED_EDGE('',*,*,#1451,.F.);
#1924=ORIENTED_EDGE('',*,*,#1457,.F.);
#1925=ORIENTED_EDGE('',*,*,#1453,.T.);
#1926=ORIENTED_EDGE('',*,*,#1458,.T.);
#1927=ORIENTED_EDGE('',*,*,#1454,.F.);
#1928=ORIENTED_EDGE('',*,*,#1458,.F.);
#1929=ORIENTED_EDGE('',*,*,#1459,.T.);
#1930=ORIENTED_EDGE('',*,*,#1460,.T.);
#1931=ORIENTED_EDGE('',*,*,#1461,.F.);
#1932=ORIENTED_EDGE('',*,*,#1460,.F.);
#1933=ORIENTED_EDGE('',*,*,#1462,.T.);
#1934=ORIENTED_EDGE('',*,*,#1463,.T.);
#1935=ORIENTED_EDGE('',*,*,#1464,.F.);
#1936=ORIENTED_EDGE('',*,*,#1463,.F.);
#1937=ORIENTED_EDGE('',*,*,#1464,.T.);
#1938=ORIENTED_EDGE('',*,*,#1465,.T.);
#1939=ORIENTED_EDGE('',*,*,#1459,.F.);
#1940=ORIENTED_EDGE('',*,*,#1465,.F.);
#1941=ORIENTED_EDGE('',*,*,#1461,.T.);
#1942=ORIENTED_EDGE('',*,*,#1466,.T.);
#1943=ORIENTED_EDGE('',*,*,#1462,.F.);
#1944=ORIENTED_EDGE('',*,*,#1466,.F.);
#1945=ORIENTED_EDGE('',*,*,#1467,.T.);
#1946=ORIENTED_EDGE('',*,*,#1468,.T.);
#1947=ORIENTED_EDGE('',*,*,#1469,.F.);
#1948=ORIENTED_EDGE('',*,*,#1468,.F.);
#1949=ORIENTED_EDGE('',*,*,#1470,.T.);
#1950=ORIENTED_EDGE('',*,*,#1471,.T.);
#1951=ORIENTED_EDGE('',*,*,#1472,.F.);
#1952=ORIENTED_EDGE('',*,*,#1471,.F.);
#1953=ORIENTED_EDGE('',*,*,#1472,.T.);
#1954=ORIENTED_EDGE('',*,*,#1473,.T.);
#1955=ORIENTED_EDGE('',*,*,#1467,.F.);
#1956=ORIENTED_EDGE('',*,*,#1473,.F.);
#1957=ORIENTED_EDGE('',*,*,#1469,.T.);
#1958=ORIENTED_EDGE('',*,*,#1474,.T.);
#1959=ORIENTED_EDGE('',*,*,#1470,.F.);
#1960=ORIENTED_EDGE('',*,*,#1474,.F.);
#1961=ORIENTED_EDGE('',*,*,#1475,.T.);
#1962=ORIENTED_EDGE('',*,*,#1476,.T.);
#1963=ORIENTED_EDGE('',*,*,#1477,.F.);
#1964=ORIENTED_EDGE('',*,*,#1476,.F.);
#1965=ORIENTED_EDGE('',*,*,#1478,.T.);
#1966=ORIENTED_EDGE('',*,*,#1479,.T.);
#1967=ORIENTED_EDGE('',*,*,#1480,.F.);
#1968=ORIENTED_EDGE('',*,*,#1479,.F.);
#1969=ORIENTED_EDGE('',*,*,#1480,.T.);
#1970=ORIENTED_EDGE('',*,*,#1481,.T.);
#1971=ORIENTED_EDGE('',*,*,#1475,.F.);
#1972=ORIENTED_EDGE('',*,*,#1481,.F.);
#1973=ORIENTED_EDGE('',*,*,#1477,.T.);
#1974=ORIENTED_EDGE('',*,*,#1482,.T.);
#1975=ORIENTED_EDGE('',*,*,#1478,.F.);
#1976=ORIENTED_EDGE('',*,*,#1482,.F.);
#1977=ORIENTED_EDGE('',*,*,#1483,.T.);
#1978=ORIENTED_EDGE('',*,*,#1484,.T.);
#1979=ORIENTED_EDGE('',*,*,#1485,.F.);
#1980=ORIENTED_EDGE('',*,*,#1484,.F.);
#1981=ORIENTED_EDGE('',*,*,#1486,.T.);
#1982=ORIENTED_EDGE('',*,*,#1487,.T.);
#1983=ORIENTED_EDGE('',*,*,#1488,.F.);
#1984=ORIENTED_EDGE('',*,*,#1487,.F.);
#1985=ORIENTED_EDGE('',*,*,#1488,.T.);
#1986=ORIENTED_EDGE('',*,*,#1489,.T.);
#1987=ORIENTED_EDGE('',*,*,#1483,.F.);
#1988=ORIENTED_EDGE('',*,*,#1489,.F.);
#1989=ORIENTED_EDGE('',*,*,#1485,.T.);
#1990=ORIENTED_EDGE('',*,*,#1490,.T.);
#1991=ORIENTED_EDGE('',*,*,#1486,.F.);
#1992=ORIENTED_EDGE('',*,*,#1490,.F.);
#1993=ORIENTED_EDGE('',*,*,#1491,.T.);
#1994=ORIENTED_EDGE('',*,*,#1492,.T.);
#1995=ORIENTED_EDGE('',*,*,#1493,.F.);
#1996=ORIENTED_EDGE('',*,*,#1492,.F.);
#1997=ORIENTED_EDGE('',*,*,#1494,.T.);
#1998=ORIENTED_EDGE('',*,*,#1495,.T.);
#1999=ORIENTED_EDGE('',*,*,#1496,.F.);
#2000=ORIENTED_EDGE('',*,*,#1495,.F.);
#2001=ORIENTED_EDGE('',*,*,#1496,.T.);
#2002=ORIENTED_EDGE('',*,*,#1497,.T.);
#2003=ORIENTED_EDGE('',*,*,#1491,.F.);
#2004=ORIENTED_EDGE('',*,*,#1497,.F.);
#2005=ORIENTED_EDGE('',*,*,#1493,.T.);
#2006=ORIENTED_EDGE('',*,*,#1498,.T.);
#2007=ORIENTED_EDGE('',*,*,#1494,.F.);
#2008=ORIENTED_EDGE('',*,*,#1498,.F.);
#2009=ORIENTED_EDGE('',*,*,#1499,.T.);
#2010=ORIENTED_EDGE('',*,*,#1500,.T.);
#2011=ORIENTED_EDGE('',*,*,#1501,.F.);
#2012=ORIENTED_EDGE('',*,*,#1500,.F.);
#2013=ORIENTED_EDGE('',*,*,#1502,.T.);
#2014=ORIENTED_EDGE('',*,*,#1503,.T.);
#2015=ORIENTED_EDGE('',*,*,#1504,.F.);
#2016=ORIENTED_EDGE('',*,*,#1503,.F.);
#2017=ORIENTED_EDGE('',*,*,#1504,.T.);
#2018=ORIENTED_EDGE('',*,*,#1505,.T.);
#2019=ORIENTED_EDGE('',*,*,#1499,.F.);
#2020=ORIENTED_EDGE('',*,*,#1505,.F.);
#2021=ORIENTED_EDGE('',*,*,#1501,.T.);
#2022=ORIENTED_EDGE('',*,*,#1506,.T.);
#2023=ORIENTED_EDGE('',*,*,#1502,.F.);
#2024=ORIENTED_EDGE('',*,*,#1506,.F.);
#2025=ORIENTED_EDGE('',*,*,#1507,.T.);
#2026=ORIENTED_EDGE('',*,*,#1508,.T.);
#2027=ORIENTED_EDGE('',*,*,#1509,.F.);
#2028=ORIENTED_EDGE('',*,*,#1508,.F.);
#2029=ORIENTED_EDGE('',*,*,#1510,.T.);
#2030=ORIENTED_EDGE('',*,*,#1511,.T.);
#2031=ORIENTED_EDGE('',*,*,#1512,.F.);
#2032=ORIENTED_EDGE('',*,*,#1511,.F.);
#2033=ORIENTED_EDGE('',*,*,#1512,.T.);
#2034=ORIENTED_EDGE('',*,*,#1513,.T.);
#2035=ORIENTED_EDGE('',*,*,#1507,.F.);
#2036=ORIENTED_EDGE('',*,*,#1513,.F.);
#2037=ORIENTED_EDGE('',*,*,#1509,.T.);
#2038=ORIENTED_EDGE('',*,*,#1514,.T.);
#2039=ORIENTED_EDGE('',*,*,#1510,.F.);
#2040=ORIENTED_EDGE('',*,*,#1514,.F.);
#2041=ORIENTED_EDGE('',*,*,#1515,.T.);
#2042=ORIENTED_EDGE('',*,*,#1516,.T.);
#2043=ORIENTED_EDGE('',*,*,#1517,.F.);
#2044=ORIENTED_EDGE('',*,*,#1516,.F.);
#2045=ORIENTED_EDGE('',*,*,#1518,.T.);
#2046=ORIENTED_EDGE('',*,*,#1519,.T.);
#2047=ORIENTED_EDGE('',*,*,#1520,.F.);
#2048=ORIENTED_EDGE('',*,*,#1519,.F.);
#2049=ORIENTED_EDGE('',*,*,#1520,.T.);
#2050=ORIENTED_EDGE('',*,*,#1521,.T.);
#2051=ORIENTED_EDGE('',*,*,#1515,.F.);
#2052=ORIENTED_EDGE('',*,*,#1521,.F.);
#2053=ORIENTED_EDGE('',*,*,#1517,.T.);
#2054=ORIENTED_EDGE('',*,*,#1522,.T.);
#2055=ORIENTED_EDGE('',*,*,#1518,.F.);
#2056=ORIENTED_EDGE('',*,*,#1522,.F.);
#2057=ORIENTED_EDGE('',*,*,#1523,.T.);
#2058=ORIENTED_EDGE('',*,*,#1524,.T.);
#2059=ORIENTED_EDGE('',*,*,#1525,.T.);
#2060=ORIENTED_EDGE('',*,*,#1524,.F.);
#2061=ORIENTED_EDGE('',*,*,#1526,.T.);
#2062=ORIENTED_EDGE('',*,*,#1527,.T.);
#2063=ORIENTED_EDGE('',*,*,#1528,.T.);
#2064=ORIENTED_EDGE('',*,*,#1527,.F.);
#2065=ORIENTED_EDGE('',*,*,#1529,.T.);
#2066=ORIENTED_EDGE('',*,*,#1530,.T.);
#2067=ORIENTED_EDGE('',*,*,#1531,.T.);
#2068=ORIENTED_EDGE('',*,*,#1530,.F.);
#2069=ORIENTED_EDGE('',*,*,#1532,.T.);
#2070=ORIENTED_EDGE('',*,*,#1533,.T.);
#2071=ORIENTED_EDGE('',*,*,#1534,.T.);
#2072=ORIENTED_EDGE('',*,*,#1533,.F.);
#2073=ORIENTED_EDGE('',*,*,#1535,.F.);
#2074=ORIENTED_EDGE('',*,*,#1536,.T.);
#2075=ORIENTED_EDGE('',*,*,#1532,.F.);
#2076=ORIENTED_EDGE('',*,*,#1536,.F.);
#2077=ORIENTED_EDGE('',*,*,#1537,.F.);
#2078=ORIENTED_EDGE('',*,*,#1538,.T.);
#2079=ORIENTED_EDGE('',*,*,#1529,.F.);
#2080=ORIENTED_EDGE('',*,*,#1538,.F.);
#2081=ORIENTED_EDGE('',*,*,#1539,.F.);
#2082=ORIENTED_EDGE('',*,*,#1540,.T.);
#2083=ORIENTED_EDGE('',*,*,#1526,.F.);
#2084=ORIENTED_EDGE('',*,*,#1540,.F.);
#2085=ORIENTED_EDGE('',*,*,#1541,.F.);
#2086=ORIENTED_EDGE('',*,*,#1542,.T.);
#2087=ORIENTED_EDGE('',*,*,#1523,.F.);
#2088=ORIENTED_EDGE('',*,*,#1542,.F.);
#2089=ORIENTED_EDGE('',*,*,#1543,.F.);
#2090=ORIENTED_EDGE('',*,*,#1544,.F.);
#2091=ORIENTED_EDGE('',*,*,#1545,.F.);
#2092=ORIENTED_EDGE('',*,*,#1546,.T.);
#2093=ORIENTED_EDGE('',*,*,#1547,.F.);
#2094=ORIENTED_EDGE('',*,*,#1548,.F.);
#2095=ORIENTED_EDGE('',*,*,#1549,.F.);
#2096=ORIENTED_EDGE('',*,*,#1550,.T.);
#2097=ORIENTED_EDGE('',*,*,#1551,.F.);
#2098=ORIENTED_EDGE('',*,*,#1552,.F.);
#2099=ORIENTED_EDGE('',*,*,#1553,.F.);
#2100=ORIENTED_EDGE('',*,*,#1554,.F.);
#2101=ORIENTED_EDGE('',*,*,#1555,.T.);
#2102=ORIENTED_EDGE('',*,*,#1556,.T.);
#2103=ORIENTED_EDGE('',*,*,#1557,.T.);
#2104=ORIENTED_EDGE('',*,*,#1558,.T.);
#2105=ORIENTED_EDGE('',*,*,#1535,.T.);
#2106=ORIENTED_EDGE('',*,*,#1537,.T.);
#2107=ORIENTED_EDGE('',*,*,#1539,.T.);
#2108=ORIENTED_EDGE('',*,*,#1541,.T.);
#2109=ORIENTED_EDGE('',*,*,#1551,.T.);
#2110=ORIENTED_EDGE('',*,*,#1559,.F.);
#2111=ORIENTED_EDGE('',*,*,#1560,.F.);
#2112=ORIENTED_EDGE('',*,*,#1546,.F.);
#2113=ORIENTED_EDGE('',*,*,#1561,.F.);
#2114=ORIENTED_EDGE('',*,*,#1548,.T.);
#2115=ORIENTED_EDGE('',*,*,#1562,.F.);
#2116=ORIENTED_EDGE('',*,*,#1563,.T.);
#2117=ORIENTED_EDGE('',*,*,#1553,.T.);
#2118=ORIENTED_EDGE('',*,*,#1564,.F.);
#2119=ORIENTED_EDGE('',*,*,#1565,.F.);
#2120=ORIENTED_EDGE('',*,*,#1550,.F.);
#2121=ORIENTED_EDGE('',*,*,#1566,.F.);
#2122=ORIENTED_EDGE('',*,*,#1544,.T.);
#2123=ORIENTED_EDGE('',*,*,#1567,.F.);
#2124=ORIENTED_EDGE('',*,*,#1568,.T.);
#2125=ORIENTED_EDGE('',*,*,#1555,.F.);
#2126=ORIENTED_EDGE('',*,*,#1569,.F.);
#2127=ORIENTED_EDGE('',*,*,#1570,.T.);
#2128=ORIENTED_EDGE('',*,*,#1571,.T.);
#2129=ORIENTED_EDGE('',*,*,#1556,.F.);
#2130=ORIENTED_EDGE('',*,*,#1571,.F.);
#2131=ORIENTED_EDGE('',*,*,#1572,.T.);
#2132=ORIENTED_EDGE('',*,*,#1573,.T.);
#2133=ORIENTED_EDGE('',*,*,#1557,.F.);
#2134=ORIENTED_EDGE('',*,*,#1573,.F.);
#2135=ORIENTED_EDGE('',*,*,#1574,.T.);
#2136=ORIENTED_EDGE('',*,*,#1575,.T.);
#2137=ORIENTED_EDGE('',*,*,#1558,.F.);
#2138=ORIENTED_EDGE('',*,*,#1575,.F.);
#2139=ORIENTED_EDGE('',*,*,#1576,.T.);
#2140=ORIENTED_EDGE('',*,*,#1569,.T.);
#2141=ORIENTED_EDGE('',*,*,#1572,.F.);
#2142=ORIENTED_EDGE('',*,*,#1570,.F.);
#2143=ORIENTED_EDGE('',*,*,#1576,.F.);
#2144=ORIENTED_EDGE('',*,*,#1574,.F.);
#2145=ORIENTED_EDGE('',*,*,#1561,.T.);
#2146=ORIENTED_EDGE('',*,*,#1545,.T.);
#2147=ORIENTED_EDGE('',*,*,#1566,.T.);
#2148=ORIENTED_EDGE('',*,*,#1549,.T.);
#2149=ORIENTED_EDGE('',*,*,#1552,.T.);
#2150=ORIENTED_EDGE('',*,*,#1563,.F.);
#2151=ORIENTED_EDGE('',*,*,#1577,.F.);
#2152=ORIENTED_EDGE('',*,*,#1564,.T.);
#2153=ORIENTED_EDGE('',*,*,#1547,.T.);
#2154=ORIENTED_EDGE('',*,*,#1565,.T.);
#2155=ORIENTED_EDGE('',*,*,#1577,.T.);
#2156=ORIENTED_EDGE('',*,*,#1562,.T.);
#2157=ORIENTED_EDGE('',*,*,#1531,.F.);
#2158=ORIENTED_EDGE('',*,*,#1534,.F.);
#2159=ORIENTED_EDGE('',*,*,#1554,.T.);
#2160=ORIENTED_EDGE('',*,*,#1568,.F.);
#2161=ORIENTED_EDGE('',*,*,#1578,.F.);
#2162=ORIENTED_EDGE('',*,*,#1559,.T.);
#2163=ORIENTED_EDGE('',*,*,#1567,.T.);
#2164=ORIENTED_EDGE('',*,*,#1543,.T.);
#2165=ORIENTED_EDGE('',*,*,#1560,.T.);
#2166=ORIENTED_EDGE('',*,*,#1578,.T.);
#2167=ORIENTED_EDGE('',*,*,#1525,.F.);
#2168=ORIENTED_EDGE('',*,*,#1528,.F.);
#2169=ORIENTED_EDGE('',*,*,#1579,.T.);
#2170=ORIENTED_EDGE('',*,*,#1580,.T.);
#2171=ORIENTED_EDGE('',*,*,#1581,.T.);
#2172=ORIENTED_EDGE('',*,*,#1582,.T.);
#2173=ORIENTED_EDGE('',*,*,#1583,.T.);
#2174=ORIENTED_EDGE('',*,*,#1584,.T.);
#2175=ORIENTED_EDGE('',*,*,#1585,.T.);
#2176=ORIENTED_EDGE('',*,*,#1579,.F.);
#2177=ORIENTED_EDGE('',*,*,#1586,.F.);
#2178=ORIENTED_EDGE('',*,*,#1587,.T.);
#2179=ORIENTED_EDGE('',*,*,#1588,.F.);
#2180=ORIENTED_EDGE('',*,*,#1587,.F.);
#2181=ORIENTED_EDGE('',*,*,#1589,.F.);
#2182=ORIENTED_EDGE('',*,*,#1590,.T.);
#2183=ORIENTED_EDGE('',*,*,#1591,.T.);
#2184=ORIENTED_EDGE('',*,*,#1590,.F.);
#2185=ORIENTED_EDGE('',*,*,#1588,.T.);
#2186=ORIENTED_EDGE('',*,*,#1592,.T.);
#2187=ORIENTED_EDGE('',*,*,#1589,.T.);
#2188=ORIENTED_EDGE('',*,*,#1592,.F.);
#2189=ORIENTED_EDGE('',*,*,#1593,.F.);
#2190=ORIENTED_EDGE('',*,*,#1594,.T.);
#2191=ORIENTED_EDGE('',*,*,#1595,.T.);
#2192=ORIENTED_EDGE('',*,*,#1594,.F.);
#2193=ORIENTED_EDGE('',*,*,#1593,.T.);
#2194=ORIENTED_EDGE('',*,*,#1596,.F.);
#2195=ORIENTED_EDGE('',*,*,#1596,.T.);
#2196=ORIENTED_EDGE('',*,*,#1597,.T.);
#2197=ORIENTED_EDGE('',*,*,#1598,.T.);
#2198=ORIENTED_EDGE('',*,*,#1599,.T.);
#2199=ORIENTED_EDGE('',*,*,#1600,.T.);
#2200=ORIENTED_EDGE('',*,*,#1601,.T.);
#2201=ORIENTED_EDGE('',*,*,#1602,.T.);
#2202=ORIENTED_EDGE('',*,*,#1595,.F.);
#2203=ORIENTED_EDGE('',*,*,#1586,.T.);
#2204=ORIENTED_EDGE('',*,*,#1591,.F.);
#2205=ORIENTED_EDGE('',*,*,#1603,.T.);
#2206=ORIENTED_EDGE('',*,*,#1604,.T.);
#2207=ORIENTED_EDGE('',*,*,#1605,.T.);
#2208=ORIENTED_EDGE('',*,*,#1598,.F.);
#2209=ORIENTED_EDGE('',*,*,#1606,.F.);
#2210=ORIENTED_EDGE('',*,*,#1607,.T.);
#2211=ORIENTED_EDGE('',*,*,#1608,.T.);
#2212=ORIENTED_EDGE('',*,*,#1609,.T.);
#2213=ORIENTED_EDGE('',*,*,#1599,.F.);
#2214=ORIENTED_EDGE('',*,*,#1605,.F.);
#2215=ORIENTED_EDGE('',*,*,#1610,.T.);
#2216=ORIENTED_EDGE('',*,*,#1611,.T.);
#2217=ORIENTED_EDGE('',*,*,#1612,.T.);
#2218=ORIENTED_EDGE('',*,*,#1600,.F.);
#2219=ORIENTED_EDGE('',*,*,#1609,.F.);
#2220=ORIENTED_EDGE('',*,*,#1613,.T.);
#2221=ORIENTED_EDGE('',*,*,#1614,.T.);
#2222=ORIENTED_EDGE('',*,*,#1615,.T.);
#2223=ORIENTED_EDGE('',*,*,#1601,.F.);
#2224=ORIENTED_EDGE('',*,*,#1612,.F.);
#2225=ORIENTED_EDGE('',*,*,#1616,.T.);
#2226=ORIENTED_EDGE('',*,*,#1617,.T.);
#2227=ORIENTED_EDGE('',*,*,#1618,.T.);
#2228=ORIENTED_EDGE('',*,*,#1602,.F.);
#2229=ORIENTED_EDGE('',*,*,#1615,.F.);
#2230=ORIENTED_EDGE('',*,*,#1619,.T.);
#2231=ORIENTED_EDGE('',*,*,#1620,.T.);
#2232=ORIENTED_EDGE('',*,*,#1606,.T.);
#2233=ORIENTED_EDGE('',*,*,#1597,.F.);
#2234=ORIENTED_EDGE('',*,*,#1618,.F.);
#2235=ORIENTED_EDGE('',*,*,#1585,.F.);
#2236=ORIENTED_EDGE('',*,*,#1613,.F.);
#2237=ORIENTED_EDGE('',*,*,#1611,.F.);
#2238=ORIENTED_EDGE('',*,*,#1584,.F.);
#2239=ORIENTED_EDGE('',*,*,#1616,.F.);
#2240=ORIENTED_EDGE('',*,*,#1614,.F.);
#2241=ORIENTED_EDGE('',*,*,#1583,.F.);
#2242=ORIENTED_EDGE('',*,*,#1619,.F.);
#2243=ORIENTED_EDGE('',*,*,#1617,.F.);
#2244=ORIENTED_EDGE('',*,*,#1582,.F.);
#2245=ORIENTED_EDGE('',*,*,#1603,.F.);
#2246=ORIENTED_EDGE('',*,*,#1620,.F.);
#2247=ORIENTED_EDGE('',*,*,#1581,.F.);
#2248=ORIENTED_EDGE('',*,*,#1607,.F.);
#2249=ORIENTED_EDGE('',*,*,#1604,.F.);
#2250=ORIENTED_EDGE('',*,*,#1580,.F.);
#2251=ORIENTED_EDGE('',*,*,#1610,.F.);
#2252=ORIENTED_EDGE('',*,*,#1608,.F.);
#2253=CONICAL_SURFACE('',#2536,2.,1.02974426);
#2254=CONICAL_SURFACE('',#2540,2.,1.02974426);
#2255=CONICAL_SURFACE('',#2544,2.,1.02974426);
#2256=CONICAL_SURFACE('',#2548,2.,1.02974426);
#2257=CONICAL_SURFACE('',#2817,1732.05080756886,1.04719755119659);
#2258=CONICAL_SURFACE('',#2828,1.61,0.785398163397447);
#2259=ADVANCED_FACE('',(#308),#2253,.F.);
#2260=ADVANCED_FACE('',(#309),#255,.F.);
#2261=ADVANCED_FACE('',(#310),#2254,.F.);
#2262=ADVANCED_FACE('',(#311),#256,.F.);
#2263=ADVANCED_FACE('',(#312),#2255,.F.);
#2264=ADVANCED_FACE('',(#313),#257,.F.);
#2265=ADVANCED_FACE('',(#314),#2256,.F.);
#2266=ADVANCED_FACE('',(#315),#258,.F.);
#2267=ADVANCED_FACE('',(#316),#259,.F.);
#2268=ADVANCED_FACE('',(#317),#260,.F.);
#2269=ADVANCED_FACE('',(#318),#261,.F.);
#2270=ADVANCED_FACE('',(#319,#157),#191,.F.);
#2271=ADVANCED_FACE('',(#320,#158),#192,.T.);
#2272=ADVANCED_FACE('',(#321),#193,.F.);
#2273=ADVANCED_FACE('',(#322,#159,#160,#161,#162,#163),#194,.F.);
#2274=ADVANCED_FACE('',(#323),#195,.F.);
#2275=ADVANCED_FACE('',(#324),#196,.F.);
#2276=ADVANCED_FACE('',(#325),#197,.T.);
#2277=ADVANCED_FACE('',(#326),#198,.T.);
#2278=ADVANCED_FACE('',(#327),#199,.T.);
#2279=ADVANCED_FACE('',(#328),#262,.F.);
#2280=ADVANCED_FACE('',(#329),#263,.T.);
#2281=ADVANCED_FACE('',(#330),#264,.T.);
#2282=ADVANCED_FACE('',(#331),#265,.T.);
#2283=ADVANCED_FACE('',(#332,#164),#200,.T.);
#2284=ADVANCED_FACE('',(#333),#201,.F.);
#2285=ADVANCED_FACE('',(#334,#165),#202,.F.);
#2286=ADVANCED_FACE('',(#335,#166),#203,.T.);
#2287=ADVANCED_FACE('',(#336),#204,.T.);
#2288=ADVANCED_FACE('',(#337),#266,.F.);
#2289=ADVANCED_FACE('',(#338),#267,.T.);
#2290=ADVANCED_FACE('',(#339,#167),#205,.F.);
#2291=ADVANCED_FACE('',(#340),#206,.F.);
#2292=ADVANCED_FACE('',(#341),#207,.T.);
#2293=ADVANCED_FACE('',(#342),#95,.T.);
#2294=ADVANCED_FACE('',(#343),#208,.T.);
#2295=ADVANCED_FACE('',(#344),#209,.F.);
#2296=ADVANCED_FACE('',(#345),#96,.T.);
#2297=ADVANCED_FACE('',(#346),#210,.F.);
#2298=ADVANCED_FACE('',(#347),#268,.F.);
#2299=ADVANCED_FACE('',(#348),#269,.F.);
#2300=ADVANCED_FACE('',(#349),#270,.F.);
#2301=ADVANCED_FACE('',(#350),#271,.F.);
#2302=ADVANCED_FACE('',(#351),#272,.F.);
#2303=ADVANCED_FACE('',(#352,#168,#169,#170,#171,#172),#211,.T.);
#2304=ADVANCED_FACE('',(#353,#173,#174,#175,#176,#177),#212,.F.);
#2305=ADVANCED_FACE('',(#354),#213,.F.);
#2306=ADVANCED_FACE('',(#355),#214,.F.);
#2307=ADVANCED_FACE('',(#356),#215,.F.);
#2308=ADVANCED_FACE('',(#357),#216,.F.);
#2309=ADVANCED_FACE('',(#358),#273,.F.);
#2310=ADVANCED_FACE('',(#359),#274,.T.);
#2311=ADVANCED_FACE('',(#360,#178),#217,.F.);
#2312=ADVANCED_FACE('',(#361),#275,.T.);
#2313=ADVANCED_FACE('',(#362),#218,.F.);
#2314=ADVANCED_FACE('',(#363),#219,.F.);
#2315=ADVANCED_FACE('',(#364),#220,.F.);
#2316=ADVANCED_FACE('',(#365),#221,.T.);
#2317=ADVANCED_FACE('',(#366),#60,.T.);
#2318=ADVANCED_FACE('',(#367),#61,.T.);
#2319=ADVANCED_FACE('',(#368),#276,.T.);
#2320=ADVANCED_FACE('',(#369),#277,.T.);
#2321=ADVANCED_FACE('',(#370),#62,.T.);
#2322=ADVANCED_FACE('',(#371),#63,.T.);
#2323=ADVANCED_FACE('',(#372),#278,.T.);
#2324=ADVANCED_FACE('',(#373),#279,.T.);
#2325=ADVANCED_FACE('',(#374),#64,.T.);
#2326=ADVANCED_FACE('',(#375),#65,.T.);
#2327=ADVANCED_FACE('',(#376),#280,.T.);
#2328=ADVANCED_FACE('',(#377),#281,.T.);
#2329=ADVANCED_FACE('',(#378),#66,.T.);
#2330=ADVANCED_FACE('',(#379),#67,.T.);
#2331=ADVANCED_FACE('',(#380),#282,.T.);
#2332=ADVANCED_FACE('',(#381),#283,.T.);
#2333=ADVANCED_FACE('',(#382),#68,.T.);
#2334=ADVANCED_FACE('',(#383),#69,.T.);
#2335=ADVANCED_FACE('',(#384),#284,.T.);
#2336=ADVANCED_FACE('',(#385),#285,.T.);
#2337=ADVANCED_FACE('',(#386),#70,.T.);
#2338=ADVANCED_FACE('',(#387),#71,.T.);
#2339=ADVANCED_FACE('',(#388),#286,.T.);
#2340=ADVANCED_FACE('',(#389),#287,.T.);
#2341=ADVANCED_FACE('',(#390),#72,.T.);
#2342=ADVANCED_FACE('',(#391),#73,.T.);
#2343=ADVANCED_FACE('',(#392),#288,.T.);
#2344=ADVANCED_FACE('',(#393),#289,.T.);
#2345=ADVANCED_FACE('',(#394),#74,.T.);
#2346=ADVANCED_FACE('',(#395),#75,.T.);
#2347=ADVANCED_FACE('',(#396),#290,.T.);
#2348=ADVANCED_FACE('',(#397),#291,.T.);
#2349=ADVANCED_FACE('',(#398),#76,.T.);
#2350=ADVANCED_FACE('',(#399),#77,.T.);
#2351=ADVANCED_FACE('',(#400),#292,.T.);
#2352=ADVANCED_FACE('',(#401),#293,.T.);
#2353=ADVANCED_FACE('',(#402),#78,.T.);
#2354=ADVANCED_FACE('',(#403),#79,.T.);
#2355=ADVANCED_FACE('',(#404),#294,.T.);
#2356=ADVANCED_FACE('',(#405),#295,.T.);
#2357=ADVANCED_FACE('',(#406),#80,.T.);
#2358=ADVANCED_FACE('',(#407),#81,.T.);
#2359=ADVANCED_FACE('',(#408),#296,.T.);
#2360=ADVANCED_FACE('',(#409),#297,.T.);
#2361=ADVANCED_FACE('',(#410),#82,.T.);
#2362=ADVANCED_FACE('',(#411),#83,.T.);
#2363=ADVANCED_FACE('',(#412),#298,.T.);
#2364=ADVANCED_FACE('',(#413),#299,.T.);
#2365=ADVANCED_FACE('',(#414),#84,.T.);
#2366=ADVANCED_FACE('',(#415),#85,.T.);
#2367=ADVANCED_FACE('',(#416),#300,.T.);
#2368=ADVANCED_FACE('',(#417),#301,.T.);
#2369=ADVANCED_FACE('',(#418),#86,.T.);
#2370=ADVANCED_FACE('',(#419),#87,.T.);
#2371=ADVANCED_FACE('',(#420),#88,.T.);
#2372=ADVANCED_FACE('',(#421),#89,.T.);
#2373=ADVANCED_FACE('',(#422),#302,.F.);
#2374=ADVANCED_FACE('',(#423),#303,.F.);
#2375=ADVANCED_FACE('',(#424),#304,.F.);
#2376=ADVANCED_FACE('',(#425),#305,.F.);
#2377=ADVANCED_FACE('',(#426),#222,.F.);
#2378=ADVANCED_FACE('',(#427),#223,.F.);
#2379=ADVANCED_FACE('',(#428,#179,#180,#181,#182,#183),#224,.F.);
#2380=ADVANCED_FACE('',(#429),#225,.F.);
#2381=ADVANCED_FACE('',(#430),#226,.F.);
#2382=ADVANCED_FACE('',(#431),#227,.T.);
#2383=ADVANCED_FACE('',(#432),#228,.T.);
#2384=ADVANCED_FACE('',(#433),#229,.T.);
#2385=ADVANCED_FACE('',(#434),#230,.T.);
#2386=ADVANCED_FACE('',(#435),#231,.T.);
#2387=ADVANCED_FACE('',(#436),#232,.F.);
#2388=ADVANCED_FACE('',(#437),#233,.F.);
#2389=ADVANCED_FACE('',(#438,#184,#185),#234,.F.);
#2390=ADVANCED_FACE('',(#439),#235,.F.);
#2391=ADVANCED_FACE('',(#440,#186,#187),#236,.F.);
#2392=ADVANCED_FACE('',(#441),#2257,.F.);
#2393=ADVANCED_FACE('',(#442),#90,.F.);
#2394=ADVANCED_FACE('',(#443),#2258,.T.);
#2395=ADVANCED_FACE('',(#444),#306,.T.);
#2396=ADVANCED_FACE('',(#445),#307,.T.);
#2397=ADVANCED_FACE('',(#446,#188),#59,.T.);
#2398=ADVANCED_FACE('',(#447,#189),#237,.T.);
#2399=ADVANCED_FACE('',(#448,#190),#238,.F.);
#2400=ADVANCED_FACE('',(#449),#239,.F.);
#2401=ADVANCED_FACE('',(#450),#240,.T.);
#2402=ADVANCED_FACE('',(#451),#241,.T.);
#2403=ADVANCED_FACE('',(#452),#242,.T.);
#2404=ADVANCED_FACE('',(#453),#243,.T.);
#2405=ADVANCED_FACE('',(#454),#244,.T.);
#2406=ADVANCED_FACE('',(#455),#245,.T.);
#2407=ADVANCED_FACE('',(#456),#246,.F.);
#2408=ADVANCED_FACE('',(#457),#247,.F.);
#2409=ADVANCED_FACE('',(#458),#248,.F.);
#2410=ADVANCED_FACE('',(#459),#249,.F.);
#2411=ADVANCED_FACE('',(#460),#250,.F.);
#2412=ADVANCED_FACE('',(#461),#251,.F.);
#2413=CLOSED_SHELL('',(#2259,#2260,#2261,#2262,#2263,#2264,#2265,#2266,
#2267,#2268,#2269,#2270,#2271,#2272,#2273,#2274,#2275,#2276,#2277,#2278));
#2414=CLOSED_SHELL('',(#2279,#2280,#2281,#2282,#2283,#2284,#2285,#2286,
#2287));
#2415=CLOSED_SHELL('',(#2288,#2289,#2290,#2291,#2292));
#2416=CLOSED_SHELL('',(#2293,#2294,#2295,#2296,#2297));
#2417=CLOSED_SHELL('',(#2298,#2299,#2300,#2301,#2302,#2303,#2304,#2305,
#2306,#2307,#2308));
#2418=CLOSED_SHELL('',(#2309,#2310,#2311,#2312,#2313,#2314,#2315,#2316));
#2419=CLOSED_SHELL('',(#2317,#2318,#2319,#2320));
#2420=CLOSED_SHELL('',(#2321,#2322,#2323,#2324));
#2421=CLOSED_SHELL('',(#2325,#2326,#2327,#2328));
#2422=CLOSED_SHELL('',(#2329,#2330,#2331,#2332));
#2423=CLOSED_SHELL('',(#2333,#2334,#2335,#2336));
#2424=CLOSED_SHELL('',(#2337,#2338,#2339,#2340));
#2425=CLOSED_SHELL('',(#2341,#2342,#2343,#2344));
#2426=CLOSED_SHELL('',(#2345,#2346,#2347,#2348));
#2427=CLOSED_SHELL('',(#2349,#2350,#2351,#2352));
#2428=CLOSED_SHELL('',(#2353,#2354,#2355,#2356));
#2429=CLOSED_SHELL('',(#2357,#2358,#2359,#2360));
#2430=CLOSED_SHELL('',(#2361,#2362,#2363,#2364));
#2431=CLOSED_SHELL('',(#2365,#2366,#2367,#2368));
#2432=CLOSED_SHELL('',(#2369,#2370,#2371,#2372,#2373,#2374,#2375,#2376,
#2377,#2378,#2379,#2380,#2381,#2382,#2383,#2384,#2385,#2386,#2387,#2388,
#2389,#2390,#2391));
#2433=CLOSED_SHELL('',(#2392,#2393,#2394,#2395,#2396,#2397,#2398,#2399,
#2400,#2401,#2402,#2403,#2404,#2405,#2406,#2407,#2408,#2409,#2410,#2411,
#2412));
#2434=DERIVED_UNIT_ELEMENT(#2452,1.);
#2435=DERIVED_UNIT_ELEMENT(#7629,-3.);
#2436=DERIVED_UNIT_ELEMENT(#2452,1.);
#2437=DERIVED_UNIT_ELEMENT(#7629,-3.);
#2438=DERIVED_UNIT_ELEMENT(#2452,1.);
#2439=DERIVED_UNIT_ELEMENT(#7629,-3.);
#2440=DERIVED_UNIT_ELEMENT(#2452,1.);
#2441=DERIVED_UNIT_ELEMENT(#7629,-3.);
#2442=DERIVED_UNIT_ELEMENT(#2452,1.);
#2443=DERIVED_UNIT_ELEMENT(#7629,-3.);
#2444=DERIVED_UNIT_ELEMENT(#2452,1.);
#2445=DERIVED_UNIT_ELEMENT(#7629,-3.);
#2446=DERIVED_UNIT_ELEMENT(#2452,1.);
#2447=DERIVED_UNIT_ELEMENT(#7629,-3.);
#2448=DERIVED_UNIT_ELEMENT(#2452,1.);
#2449=DERIVED_UNIT_ELEMENT(#7629,-3.);
#2450=DERIVED_UNIT_ELEMENT(#2452,1.);
#2451=DERIVED_UNIT_ELEMENT(#7629,-3.);
#2452=(
MASS_UNIT()
NAMED_UNIT(*)
SI_UNIT(.KILO.,.GRAM.)
);
#2453=DERIVED_UNIT((#2434,#2435));
#2454=DERIVED_UNIT((#2436,#2437));
#2455=DERIVED_UNIT((#2438,#2439));
#2456=DERIVED_UNIT((#2440,#2441));
#2457=DERIVED_UNIT((#2442,#2443));
#2458=DERIVED_UNIT((#2444,#2445));
#2459=DERIVED_UNIT((#2446,#2447));
#2460=DERIVED_UNIT((#2448,#2449));
#2461=DERIVED_UNIT((#2450,#2451));
#2462=MEASURE_REPRESENTATION_ITEM('density measure',
POSITIVE_RATIO_MEASURE(7850.),#2453);
#2463=MEASURE_REPRESENTATION_ITEM('density measure',
POSITIVE_RATIO_MEASURE(7850.),#2454);
#2464=MEASURE_REPRESENTATION_ITEM('density measure',
POSITIVE_RATIO_MEASURE(7850.),#2455);
#2465=MEASURE_REPRESENTATION_ITEM('density measure',
POSITIVE_RATIO_MEASURE(7850.),#2456);
#2466=MEASURE_REPRESENTATION_ITEM('density measure',
POSITIVE_RATIO_MEASURE(7850.),#2457);
#2467=MEASURE_REPRESENTATION_ITEM('density measure',
POSITIVE_RATIO_MEASURE(7850.),#2458);
#2468=MEASURE_REPRESENTATION_ITEM('density measure',
POSITIVE_RATIO_MEASURE(7850.),#2459);
#2469=MEASURE_REPRESENTATION_ITEM('density measure',
POSITIVE_RATIO_MEASURE(7850.),#2460);
#2470=MEASURE_REPRESENTATION_ITEM('density measure',
POSITIVE_RATIO_MEASURE(7850.),#2461);
#2471=PROPERTY_DEFINITION_REPRESENTATION(#2516,#2489);
#2472=PROPERTY_DEFINITION_REPRESENTATION(#2517,#2490);
#2473=PROPERTY_DEFINITION_REPRESENTATION(#2518,#2491);
#2474=PROPERTY_DEFINITION_REPRESENTATION(#2519,#2492);
#2475=PROPERTY_DEFINITION_REPRESENTATION(#2520,#2493);
#2476=PROPERTY_DEFINITION_REPRESENTATION(#2521,#2494);
#2477=PROPERTY_DEFINITION_REPRESENTATION(#2522,#2495);
#2478=PROPERTY_DEFINITION_REPRESENTATION(#2523,#2496);
#2479=PROPERTY_DEFINITION_REPRESENTATION(#2524,#2497);
#2480=PROPERTY_DEFINITION_REPRESENTATION(#2525,#2498);
#2481=PROPERTY_DEFINITION_REPRESENTATION(#2526,#2499);
#2482=PROPERTY_DEFINITION_REPRESENTATION(#2527,#2500);
#2483=PROPERTY_DEFINITION_REPRESENTATION(#2528,#2501);
#2484=PROPERTY_DEFINITION_REPRESENTATION(#2529,#2502);
#2485=PROPERTY_DEFINITION_REPRESENTATION(#2530,#2503);
#2486=PROPERTY_DEFINITION_REPRESENTATION(#2531,#2504);
#2487=PROPERTY_DEFINITION_REPRESENTATION(#2532,#2505);
#2488=PROPERTY_DEFINITION_REPRESENTATION(#2533,#2506);
#2489=REPRESENTATION('material name',(#2507),#7618);
#2490=REPRESENTATION('density',(#2462),#7618);
#2491=REPRESENTATION('material name',(#2508),#7619);
#2492=REPRESENTATION('density',(#2463),#7619);
#2493=REPRESENTATION('material name',(#2509),#7620);
#2494=REPRESENTATION('density',(#2464),#7620);
#2495=REPRESENTATION('material name',(#2510),#7621);
#2496=REPRESENTATION('density',(#2465),#7621);
#2497=REPRESENTATION('material name',(#2511),#7622);
#2498=REPRESENTATION('density',(#2466),#7622);
#2499=REPRESENTATION('material name',(#2512),#7623);
#2500=REPRESENTATION('density',(#2467),#7623);
#2501=REPRESENTATION('material name',(#2513),#7624);
#2502=REPRESENTATION('density',(#2468),#7624);
#2503=REPRESENTATION('material name',(#2514),#7625);
#2504=REPRESENTATION('density',(#2469),#7625);
#2505=REPRESENTATION('material name',(#2515),#7626);
#2506=REPRESENTATION('density',(#2470),#7626);
#2507=DESCRIPTIVE_REPRESENTATION_ITEM('Steel','Steel');
#2508=DESCRIPTIVE_REPRESENTATION_ITEM('Steel','Steel');
#2509=DESCRIPTIVE_REPRESENTATION_ITEM('Steel','Steel');
#2510=DESCRIPTIVE_REPRESENTATION_ITEM('Steel','Steel');
#2511=DESCRIPTIVE_REPRESENTATION_ITEM('Steel','Steel');
#2512=DESCRIPTIVE_REPRESENTATION_ITEM('Steel','Steel');
#2513=DESCRIPTIVE_REPRESENTATION_ITEM('Steel','Steel');
#2514=DESCRIPTIVE_REPRESENTATION_ITEM('Steel','Steel');
#2515=DESCRIPTIVE_REPRESENTATION_ITEM('Steel','Steel');
#2516=PROPERTY_DEFINITION('material property','material name',#7676);
#2517=PROPERTY_DEFINITION('material property','density of part',#7676);
#2518=PROPERTY_DEFINITION('material property','material name',#7677);
#2519=PROPERTY_DEFINITION('material property','density of part',#7677);
#2520=PROPERTY_DEFINITION('material property','material name',#7678);
#2521=PROPERTY_DEFINITION('material property','density of part',#7678);
#2522=PROPERTY_DEFINITION('material property','material name',#7679);
#2523=PROPERTY_DEFINITION('material property','density of part',#7679);
#2524=PROPERTY_DEFINITION('material property','material name',#7680);
#2525=PROPERTY_DEFINITION('material property','density of part',#7680);
#2526=PROPERTY_DEFINITION('material property','material name',#7681);
#2527=PROPERTY_DEFINITION('material property','density of part',#7681);
#2528=PROPERTY_DEFINITION('material property','material name',#7682);
#2529=PROPERTY_DEFINITION('material property','density of part',#7682);
#2530=PROPERTY_DEFINITION('material property','material name',#7683);
#2531=PROPERTY_DEFINITION('material property','density of part',#7683);
#2532=PROPERTY_DEFINITION('material property','material name',#7684);
#2533=PROPERTY_DEFINITION('material property','density of part',#7684);
#2534=AXIS2_PLACEMENT_3D('',#3680,#2864,#2865);
#2535=AXIS2_PLACEMENT_3D('',#3681,#2866,#2867);
#2536=AXIS2_PLACEMENT_3D('',#3682,#2868,#2869);
#2537=AXIS2_PLACEMENT_3D('',#3686,#2871,#2872);
#2538=AXIS2_PLACEMENT_3D('',#3687,#2873,#2874);
#2539=AXIS2_PLACEMENT_3D('',#3690,#2876,#2877);
#2540=AXIS2_PLACEMENT_3D('',#3691,#2878,#2879);
#2541=AXIS2_PLACEMENT_3D('',#3695,#2881,#2882);
#2542=AXIS2_PLACEMENT_3D('',#3696,#2883,#2884);
#2543=AXIS2_PLACEMENT_3D('',#3699,#2886,#2887);
#2544=AXIS2_PLACEMENT_3D('',#3700,#2888,#2889);
#2545=AXIS2_PLACEMENT_3D('',#3704,#2891,#2892);
#2546=AXIS2_PLACEMENT_3D('',#3705,#2893,#2894);
#2547=AXIS2_PLACEMENT_3D('',#3708,#2896,#2897);
#2548=AXIS2_PLACEMENT_3D('',#3709,#2898,#2899);
#2549=AXIS2_PLACEMENT_3D('',#3713,#2901,#2902);
#2550=AXIS2_PLACEMENT_3D('',#3714,#2903,#2904);
#2551=AXIS2_PLACEMENT_3D('',#3717,#2906,#2907);
#2552=AXIS2_PLACEMENT_3D('',#3718,#2908,#2909);
#2553=AXIS2_PLACEMENT_3D('',#3721,#2910,#2911);
#2554=AXIS2_PLACEMENT_3D('',#3723,#2912,#2913);
#2555=AXIS2_PLACEMENT_3D('',#3726,#2915,#2916);
#2556=AXIS2_PLACEMENT_3D('',#3727,#2917,#2918);
#2557=AXIS2_PLACEMENT_3D('',#3728,#2919,#2920);
#2558=AXIS2_PLACEMENT_3D('',#3731,#2921,#2922);
#2559=AXIS2_PLACEMENT_3D('',#3734,#2924,#2925);
#2560=AXIS2_PLACEMENT_3D('',#3737,#2928,#2929);
#2561=AXIS2_PLACEMENT_3D('',#3739,#2930,#2931);
#2562=AXIS2_PLACEMENT_3D('',#3743,#2933,#2934);
#2563=AXIS2_PLACEMENT_3D('',#3746,#2937,#2938);
#2564=AXIS2_PLACEMENT_3D('',#3755,#2943,#2944);
#2565=AXIS2_PLACEMENT_3D('',#3764,#2949,#2950);
#2566=AXIS2_PLACEMENT_3D('',#3767,#2953,#2954);
#2567=AXIS2_PLACEMENT_3D('',#3769,#2956,#2957);
#2568=AXIS2_PLACEMENT_3D('',#3771,#2959,#2960);
#2569=AXIS2_PLACEMENT_3D('',#3772,#2961,#2962);
#2570=AXIS2_PLACEMENT_3D('',#3774,#2964,#2965);
#2571=AXIS2_PLACEMENT_3D('',#3776,#2967,#2968);
#2572=AXIS2_PLACEMENT_3D('',#3777,#2969,#2970);
#2573=AXIS2_PLACEMENT_3D('',#3778,#2971,#2972);
#2574=AXIS2_PLACEMENT_3D('',#3780,#2973,#2974);
#2575=AXIS2_PLACEMENT_3D('',#3783,#2976,#2977);
#2576=AXIS2_PLACEMENT_3D('',#3784,#2978,#2979);
#2577=AXIS2_PLACEMENT_3D('',#3786,#2980,#2981);
#2578=AXIS2_PLACEMENT_3D('',#3789,#2983,#2984);
#2579=AXIS2_PLACEMENT_3D('',#3790,#2985,#2986);
#2580=AXIS2_PLACEMENT_3D('',#3792,#2987,#2988);
#2581=AXIS2_PLACEMENT_3D('',#3795,#2990,#2991);
#2582=AXIS2_PLACEMENT_3D('',#3796,#2992,#2993);
#2583=AXIS2_PLACEMENT_3D('',#3798,#2994,#2995);
#2584=AXIS2_PLACEMENT_3D('',#3801,#2997,#2998);
#2585=AXIS2_PLACEMENT_3D('',#3802,#2999,#3000);
#2586=AXIS2_PLACEMENT_3D('',#3803,#3001,#3002);
#2587=AXIS2_PLACEMENT_3D('',#3804,#3003,#3004);
#2588=AXIS2_PLACEMENT_3D('',#3805,#3005,#3006);
#2589=AXIS2_PLACEMENT_3D('',#3806,#3007,#3008);
#2590=AXIS2_PLACEMENT_3D('',#3807,#3009,#3010);
#2591=AXIS2_PLACEMENT_3D('',#3808,#3011,#3012);
#2592=AXIS2_PLACEMENT_3D('',#3810,#3013,#3014);
#2593=AXIS2_PLACEMENT_3D('',#3813,#3016,#3017);
#2594=AXIS2_PLACEMENT_3D('',#3814,#3018,#3019);
#2595=AXIS2_PLACEMENT_3D('',#3816,#3020,#3021);
#2596=AXIS2_PLACEMENT_3D('',#3819,#3023,#3024);
#2597=AXIS2_PLACEMENT_3D('',#3820,#3025,#3026);
#2598=AXIS2_PLACEMENT_3D('',#3821,#3027,#3028);
#2599=AXIS2_PLACEMENT_3D('',#3822,#3029,#3030);
#2600=AXIS2_PLACEMENT_3D('',#3823,#3031,#3032);
#2601=AXIS2_PLACEMENT_3D('',#5452,#3033,#3034);
#2602=AXIS2_PLACEMENT_3D('',#5655,#3035,#3036);
#2603=AXIS2_PLACEMENT_3D('',#5656,#3037,#3038);
#2604=AXIS2_PLACEMENT_3D('',#5659,#3040,#3041);
#2605=AXIS2_PLACEMENT_3D('',#5660,#3042,#3043);
#2606=AXIS2_PLACEMENT_3D('',#5661,#3044,#3045);
#2607=AXIS2_PLACEMENT_3D('',#7087,#3046,#3047);
#2608=AXIS2_PLACEMENT_3D('',#7088,#3048,#3049);
#2609=AXIS2_PLACEMENT_3D('',#7089,#3050,#3051);
#2610=AXIS2_PLACEMENT_3D('',#7091,#3052,#3053);
#2611=AXIS2_PLACEMENT_3D('',#7094,#3055,#3056);
#2612=AXIS2_PLACEMENT_3D('',#7095,#3057,#3058);
#2613=AXIS2_PLACEMENT_3D('',#7097,#3059,#3060);
#2614=AXIS2_PLACEMENT_3D('',#7100,#3062,#3063);
#2615=AXIS2_PLACEMENT_3D('',#7101,#3064,#3065);
#2616=AXIS2_PLACEMENT_3D('',#7103,#3066,#3067);
#2617=AXIS2_PLACEMENT_3D('',#7106,#3069,#3070);
#2618=AXIS2_PLACEMENT_3D('',#7107,#3071,#3072);
#2619=AXIS2_PLACEMENT_3D('',#7109,#3073,#3074);
#2620=AXIS2_PLACEMENT_3D('',#7112,#3076,#3077);
#2621=AXIS2_PLACEMENT_3D('',#7113,#3078,#3079);
#2622=AXIS2_PLACEMENT_3D('',#7115,#3080,#3081);
#2623=AXIS2_PLACEMENT_3D('',#7118,#3083,#3084);
#2624=AXIS2_PLACEMENT_3D('',#7119,#3085,#3086);
#2625=AXIS2_PLACEMENT_3D('',#7128,#3091,#3092);
#2626=AXIS2_PLACEMENT_3D('',#7137,#3097,#3098);
#2627=AXIS2_PLACEMENT_3D('',#7140,#3101,#3102);
#2628=AXIS2_PLACEMENT_3D('',#7142,#3104,#3105);
#2629=AXIS2_PLACEMENT_3D('',#7144,#3107,#3108);
#2630=AXIS2_PLACEMENT_3D('',#7145,#3109,#3110);
#2631=AXIS2_PLACEMENT_3D('',#7146,#3111,#3112);
#2632=AXIS2_PLACEMENT_3D('',#7148,#3113,#3114);
#2633=AXIS2_PLACEMENT_3D('',#7151,#3116,#3117);
#2634=AXIS2_PLACEMENT_3D('',#7152,#3118,#3119);
#2635=AXIS2_PLACEMENT_3D('',#7155,#3120,#3121);
#2636=AXIS2_PLACEMENT_3D('',#7159,#3123,#3124);
#2637=AXIS2_PLACEMENT_3D('',#7161,#3126,#3127);
#2638=AXIS2_PLACEMENT_3D('',#7164,#3128,#3129);
#2639=AXIS2_PLACEMENT_3D('',#7167,#3132,#3133);
#2640=AXIS2_PLACEMENT_3D('',#7171,#3135,#3136);
#2641=AXIS2_PLACEMENT_3D('',#7173,#3138,#3139);
#2642=AXIS2_PLACEMENT_3D('',#7175,#3141,#3142);
#2643=AXIS2_PLACEMENT_3D('',#7177,#3144,#3145);
#2644=AXIS2_PLACEMENT_3D('',#7178,#3146,#3147);
#2645=AXIS2_PLACEMENT_3D('',#7179,#3148,#3149);
#2646=AXIS2_PLACEMENT_3D('',#7180,#3150,#3151);
#2647=AXIS2_PLACEMENT_3D('',#7182,#3152,#3153);
#2648=AXIS2_PLACEMENT_3D('',#7184,#3154,#3155);
#2649=AXIS2_PLACEMENT_3D('',#7185,#3156,#3157);
#2650=AXIS2_PLACEMENT_3D('',#7186,#3158,#3159);
#2651=AXIS2_PLACEMENT_3D('',#7188,#3160,#3161);
#2652=AXIS2_PLACEMENT_3D('',#7190,#3162,#3163);
#2653=AXIS2_PLACEMENT_3D('',#7191,#3164,#3165);
#2654=AXIS2_PLACEMENT_3D('',#7192,#3166,#3167);
#2655=AXIS2_PLACEMENT_3D('',#7194,#3169,#3170);
#2656=AXIS2_PLACEMENT_3D('',#7196,#3172,#3173);
#2657=AXIS2_PLACEMENT_3D('',#7198,#3174,#3175);
#2658=AXIS2_PLACEMENT_3D('',#7200,#3176,#3177);
#2659=AXIS2_PLACEMENT_3D('',#7201,#3178,#3179);
#2660=AXIS2_PLACEMENT_3D('',#7202,#3180,#3181);
#2661=AXIS2_PLACEMENT_3D('',#7204,#3182,#3183);
#2662=AXIS2_PLACEMENT_3D('',#7206,#3184,#3185);
#2663=AXIS2_PLACEMENT_3D('',#7207,#3186,#3187);
#2664=AXIS2_PLACEMENT_3D('',#7208,#3188,#3189);
#2665=AXIS2_PLACEMENT_3D('',#7210,#3191,#3192);
#2666=AXIS2_PLACEMENT_3D('',#7212,#3194,#3195);
#2667=AXIS2_PLACEMENT_3D('',#7214,#3196,#3197);
#2668=AXIS2_PLACEMENT_3D('',#7216,#3198,#3199);
#2669=AXIS2_PLACEMENT_3D('',#7217,#3200,#3201);
#2670=AXIS2_PLACEMENT_3D('',#7218,#3202,#3203);
#2671=AXIS2_PLACEMENT_3D('',#7220,#3204,#3205);
#2672=AXIS2_PLACEMENT_3D('',#7222,#3206,#3207);
#2673=AXIS2_PLACEMENT_3D('',#7223,#3208,#3209);
#2674=AXIS2_PLACEMENT_3D('',#7224,#3210,#3211);
#2675=AXIS2_PLACEMENT_3D('',#7226,#3213,#3214);
#2676=AXIS2_PLACEMENT_3D('',#7228,#3216,#3217);
#2677=AXIS2_PLACEMENT_3D('',#7230,#3218,#3219);
#2678=AXIS2_PLACEMENT_3D('',#7232,#3220,#3221);
#2679=AXIS2_PLACEMENT_3D('',#7233,#3222,#3223);
#2680=AXIS2_PLACEMENT_3D('',#7234,#3224,#3225);
#2681=AXIS2_PLACEMENT_3D('',#7236,#3226,#3227);
#2682=AXIS2_PLACEMENT_3D('',#7238,#3228,#3229);
#2683=AXIS2_PLACEMENT_3D('',#7239,#3230,#3231);
#2684=AXIS2_PLACEMENT_3D('',#7240,#3232,#3233);
#2685=AXIS2_PLACEMENT_3D('',#7242,#3235,#3236);
#2686=AXIS2_PLACEMENT_3D('',#7244,#3238,#3239);
#2687=AXIS2_PLACEMENT_3D('',#7246,#3240,#3241);
#2688=AXIS2_PLACEMENT_3D('',#7248,#3242,#3243);
#2689=AXIS2_PLACEMENT_3D('',#7249,#3244,#3245);
#2690=AXIS2_PLACEMENT_3D('',#7250,#3246,#3247);
#2691=AXIS2_PLACEMENT_3D('',#7252,#3248,#3249);
#2692=AXIS2_PLACEMENT_3D('',#7254,#3250,#3251);
#2693=AXIS2_PLACEMENT_3D('',#7255,#3252,#3253);
#2694=AXIS2_PLACEMENT_3D('',#7256,#3254,#3255);
#2695=AXIS2_PLACEMENT_3D('',#7258,#3257,#3258);
#2696=AXIS2_PLACEMENT_3D('',#7260,#3260,#3261);
#2697=AXIS2_PLACEMENT_3D('',#7262,#3262,#3263);
#2698=AXIS2_PLACEMENT_3D('',#7264,#3264,#3265);
#2699=AXIS2_PLACEMENT_3D('',#7265,#3266,#3267);
#2700=AXIS2_PLACEMENT_3D('',#7266,#3268,#3269);
#2701=AXIS2_PLACEMENT_3D('',#7268,#3270,#3271);
#2702=AXIS2_PLACEMENT_3D('',#7270,#3272,#3273);
#2703=AXIS2_PLACEMENT_3D('',#7271,#3274,#3275);
#2704=AXIS2_PLACEMENT_3D('',#7272,#3276,#3277);
#2705=AXIS2_PLACEMENT_3D('',#7274,#3279,#3280);
#2706=AXIS2_PLACEMENT_3D('',#7276,#3282,#3283);
#2707=AXIS2_PLACEMENT_3D('',#7278,#3284,#3285);
#2708=AXIS2_PLACEMENT_3D('',#7280,#3286,#3287);
#2709=AXIS2_PLACEMENT_3D('',#7281,#3288,#3289);
#2710=AXIS2_PLACEMENT_3D('',#7282,#3290,#3291);
#2711=AXIS2_PLACEMENT_3D('',#7284,#3292,#3293);
#2712=AXIS2_PLACEMENT_3D('',#7286,#3294,#3295);
#2713=AXIS2_PLACEMENT_3D('',#7287,#3296,#3297);
#2714=AXIS2_PLACEMENT_3D('',#7288,#3298,#3299);
#2715=AXIS2_PLACEMENT_3D('',#7290,#3301,#3302);
#2716=AXIS2_PLACEMENT_3D('',#7292,#3304,#3305);
#2717=AXIS2_PLACEMENT_3D('',#7294,#3306,#3307);
#2718=AXIS2_PLACEMENT_3D('',#7296,#3308,#3309);
#2719=AXIS2_PLACEMENT_3D('',#7297,#3310,#3311);
#2720=AXIS2_PLACEMENT_3D('',#7298,#3312,#3313);
#2721=AXIS2_PLACEMENT_3D('',#7300,#3314,#3315);
#2722=AXIS2_PLACEMENT_3D('',#7302,#3316,#3317);
#2723=AXIS2_PLACEMENT_3D('',#7303,#3318,#3319);
#2724=AXIS2_PLACEMENT_3D('',#7304,#3320,#3321);
#2725=AXIS2_PLACEMENT_3D('',#7306,#3323,#3324);
#2726=AXIS2_PLACEMENT_3D('',#7308,#3326,#3327);
#2727=AXIS2_PLACEMENT_3D('',#7310,#3328,#3329);
#2728=AXIS2_PLACEMENT_3D('',#7312,#3330,#3331);
#2729=AXIS2_PLACEMENT_3D('',#7313,#3332,#3333);
#2730=AXIS2_PLACEMENT_3D('',#7314,#3334,#3335);
#2731=AXIS2_PLACEMENT_3D('',#7316,#3336,#3337);
#2732=AXIS2_PLACEMENT_3D('',#7318,#3338,#3339);
#2733=AXIS2_PLACEMENT_3D('',#7319,#3340,#3341);
#2734=AXIS2_PLACEMENT_3D('',#7320,#3342,#3343);
#2735=AXIS2_PLACEMENT_3D('',#7322,#3345,#3346);
#2736=AXIS2_PLACEMENT_3D('',#7324,#3348,#3349);
#2737=AXIS2_PLACEMENT_3D('',#7326,#3350,#3351);
#2738=AXIS2_PLACEMENT_3D('',#7328,#3352,#3353);
#2739=AXIS2_PLACEMENT_3D('',#7329,#3354,#3355);
#2740=AXIS2_PLACEMENT_3D('',#7330,#3356,#3357);
#2741=AXIS2_PLACEMENT_3D('',#7332,#3358,#3359);
#2742=AXIS2_PLACEMENT_3D('',#7334,#3360,#3361);
#2743=AXIS2_PLACEMENT_3D('',#7335,#3362,#3363);
#2744=AXIS2_PLACEMENT_3D('',#7336,#3364,#3365);
#2745=AXIS2_PLACEMENT_3D('',#7338,#3367,#3368);
#2746=AXIS2_PLACEMENT_3D('',#7340,#3370,#3371);
#2747=AXIS2_PLACEMENT_3D('',#7342,#3372,#3373);
#2748=AXIS2_PLACEMENT_3D('',#7344,#3374,#3375);
#2749=AXIS2_PLACEMENT_3D('',#7345,#3376,#3377);
#2750=AXIS2_PLACEMENT_3D('',#7346,#3378,#3379);
#2751=AXIS2_PLACEMENT_3D('',#7348,#3380,#3381);
#2752=AXIS2_PLACEMENT_3D('',#7350,#3382,#3383);
#2753=AXIS2_PLACEMENT_3D('',#7351,#3384,#3385);
#2754=AXIS2_PLACEMENT_3D('',#7352,#3386,#3387);
#2755=AXIS2_PLACEMENT_3D('',#7354,#3389,#3390);
#2756=AXIS2_PLACEMENT_3D('',#7356,#3392,#3393);
#2757=AXIS2_PLACEMENT_3D('',#7358,#3394,#3395);
#2758=AXIS2_PLACEMENT_3D('',#7360,#3396,#3397);
#2759=AXIS2_PLACEMENT_3D('',#7361,#3398,#3399);
#2760=AXIS2_PLACEMENT_3D('',#7362,#3400,#3401);
#2761=AXIS2_PLACEMENT_3D('',#7364,#3402,#3403);
#2762=AXIS2_PLACEMENT_3D('',#7366,#3404,#3405);
#2763=AXIS2_PLACEMENT_3D('',#7367,#3406,#3407);
#2764=AXIS2_PLACEMENT_3D('',#7368,#3408,#3409);
#2765=AXIS2_PLACEMENT_3D('',#7370,#3411,#3412);
#2766=AXIS2_PLACEMENT_3D('',#7372,#3414,#3415);
#2767=AXIS2_PLACEMENT_3D('',#7374,#3416,#3417);
#2768=AXIS2_PLACEMENT_3D('',#7376,#3418,#3419);
#2769=AXIS2_PLACEMENT_3D('',#7377,#3420,#3421);
#2770=AXIS2_PLACEMENT_3D('',#7378,#3422,#3423);
#2771=AXIS2_PLACEMENT_3D('',#7380,#3424,#3425);
#2772=AXIS2_PLACEMENT_3D('',#7382,#3426,#3427);
#2773=AXIS2_PLACEMENT_3D('',#7383,#3428,#3429);
#2774=AXIS2_PLACEMENT_3D('',#7384,#3430,#3431);
#2775=AXIS2_PLACEMENT_3D('',#7386,#3433,#3434);
#2776=AXIS2_PLACEMENT_3D('',#7388,#3436,#3437);
#2777=AXIS2_PLACEMENT_3D('',#7389,#3438,#3439);
#2778=AXIS2_PLACEMENT_3D('',#7391,#3440,#3441);
#2779=AXIS2_PLACEMENT_3D('',#7393,#3442,#3443);
#2780=AXIS2_PLACEMENT_3D('',#7394,#3444,#3445);
#2781=AXIS2_PLACEMENT_3D('',#7395,#3446,#3447);
#2782=AXIS2_PLACEMENT_3D('',#7397,#3448,#3449);
#2783=AXIS2_PLACEMENT_3D('',#7399,#3450,#3451);
#2784=AXIS2_PLACEMENT_3D('',#7400,#3452,#3453);
#2785=AXIS2_PLACEMENT_3D('',#7401,#3454,#3455);
#2786=AXIS2_PLACEMENT_3D('',#7403,#3456,#3457);
#2787=AXIS2_PLACEMENT_3D('',#7405,#3458,#3459);
#2788=AXIS2_PLACEMENT_3D('',#7406,#3460,#3461);
#2789=AXIS2_PLACEMENT_3D('',#7407,#3462,#3463);
#2790=AXIS2_PLACEMENT_3D('',#7409,#3464,#3465);
#2791=AXIS2_PLACEMENT_3D('',#7411,#3466,#3467);
#2792=AXIS2_PLACEMENT_3D('',#7412,#3468,#3469);
#2793=AXIS2_PLACEMENT_3D('',#7413,#3470,#3471);
#2794=AXIS2_PLACEMENT_3D('',#7415,#3472,#3473);
#2795=AXIS2_PLACEMENT_3D('',#7417,#3475,#3476);
#2796=AXIS2_PLACEMENT_3D('',#7419,#3477,#3478);
#2797=AXIS2_PLACEMENT_3D('',#7421,#3480,#3481);
#2798=AXIS2_PLACEMENT_3D('',#7423,#3482,#3483);
#2799=AXIS2_PLACEMENT_3D('',#7425,#3485,#3486);
#2800=AXIS2_PLACEMENT_3D('',#7427,#3487,#3488);
#2801=AXIS2_PLACEMENT_3D('',#7429,#3490,#3491);
#2802=AXIS2_PLACEMENT_3D('',#7438,#3496,#3497);
#2803=AXIS2_PLACEMENT_3D('',#7447,#3502,#3503);
#2804=AXIS2_PLACEMENT_3D('',#7464,#3512,#3513);
#2805=AXIS2_PLACEMENT_3D('',#7472,#3519,#3520);
#2806=AXIS2_PLACEMENT_3D('',#7480,#3526,#3527);
#2807=AXIS2_PLACEMENT_3D('',#7486,#3531,#3532);
#2808=AXIS2_PLACEMENT_3D('',#7490,#3535,#3536);
#2809=AXIS2_PLACEMENT_3D('',#7494,#3539,#3540);
#2810=AXIS2_PLACEMENT_3D('',#7496,#3542,#3543);
#2811=AXIS2_PLACEMENT_3D('',#7497,#3544,#3545);
#2812=AXIS2_PLACEMENT_3D('',#7498,#3546,#3547);
#2813=AXIS2_PLACEMENT_3D('',#7500,#3549,#3550);
#2814=AXIS2_PLACEMENT_3D('',#7501,#3551,#3552);
#2815=AXIS2_PLACEMENT_3D('',#7503,#3554,#3555);
#2816=AXIS2_PLACEMENT_3D('',#7504,#3556,#3557);
#2817=AXIS2_PLACEMENT_3D('',#7505,#3558,#3559);
#2818=AXIS2_PLACEMENT_3D('',#7510,#3561,#3562);
#2819=AXIS2_PLACEMENT_3D('',#7512,#3563,#3564);
#2820=AXIS2_PLACEMENT_3D('',#7514,#3565,#3566);
#2821=AXIS2_PLACEMENT_3D('',#7516,#3567,#3568);
#2822=AXIS2_PLACEMENT_3D('',#7518,#3569,#3570);
#2823=AXIS2_PLACEMENT_3D('',#7519,#3571,#3572);
#2824=AXIS2_PLACEMENT_3D('',#7520,#3573,#3574);
#2825=AXIS2_PLACEMENT_3D('',#7522,#3575,#3576);
#2826=AXIS2_PLACEMENT_3D('',#7524,#3577,#3578);
#2827=AXIS2_PLACEMENT_3D('',#7525,#3579,#3580);
#2828=AXIS2_PLACEMENT_3D('',#7526,#3581,#3582);
#2829=AXIS2_PLACEMENT_3D('',#7528,#3583,#3584);
#2830=AXIS2_PLACEMENT_3D('',#7531,#3586,#3587);
#2831=AXIS2_PLACEMENT_3D('',#7532,#3588,#3589);
#2832=AXIS2_PLACEMENT_3D('',#7534,#3591,#3592);
#2833=AXIS2_PLACEMENT_3D('',#7536,#3593,#3594);
#2834=AXIS2_PLACEMENT_3D('',#7539,#3596,#3597);
#2835=AXIS2_PLACEMENT_3D('',#7540,#3598,#3599);
#2836=AXIS2_PLACEMENT_3D('',#7542,#3600,#3601);
#2837=AXIS2_PLACEMENT_3D('',#7543,#3602,#3603);
#2838=AXIS2_PLACEMENT_3D('',#7556,#3610,#3611);
#2839=AXIS2_PLACEMENT_3D('',#7557,#3612,#3613);
#2840=AXIS2_PLACEMENT_3D('',#7558,#3614,#3615);
#2841=AXIS2_PLACEMENT_3D('',#7565,#3620,#3621);
#2842=AXIS2_PLACEMENT_3D('',#7570,#3625,#3626);
#2843=AXIS2_PLACEMENT_3D('',#7575,#3630,#3631);
#2844=AXIS2_PLACEMENT_3D('',#7580,#3635,#3636);
#2845=AXIS2_PLACEMENT_3D('',#7585,#3640,#3641);
#2846=AXIS2_PLACEMENT_3D('',#7588,#3644,#3645);
#2847=AXIS2_PLACEMENT_3D('',#7589,#3646,#3647);
#2848=AXIS2_PLACEMENT_3D('',#7590,#3648,#3649);
#2849=AXIS2_PLACEMENT_3D('',#7591,#3650,#3651);
#2850=AXIS2_PLACEMENT_3D('',#7592,#3652,#3653);
#2851=AXIS2_PLACEMENT_3D('',#7593,#3654,#3655);
#2852=AXIS2_PLACEMENT_3D('',#7594,#3656,#3657);
#2853=AXIS2_PLACEMENT_3D('',#7595,#3658,#3659);
#2854=AXIS2_PLACEMENT_3D('',#7596,#3660,#3661);
#2855=AXIS2_PLACEMENT_3D('',#7597,#3662,#3663);
#2856=AXIS2_PLACEMENT_3D('',#7598,#3664,#3665);
#2857=AXIS2_PLACEMENT_3D('',#7599,#3666,#3667);
#2858=AXIS2_PLACEMENT_3D('',#7600,#3668,#3669);
#2859=AXIS2_PLACEMENT_3D('',#7601,#3670,#3671);
#2860=AXIS2_PLACEMENT_3D('',#7602,#3672,#3673);
#2861=AXIS2_PLACEMENT_3D('',#7603,#3674,#3675);
#2862=AXIS2_PLACEMENT_3D('',#7604,#3676,#3677);
#2863=AXIS2_PLACEMENT_3D('',#7605,#3678,#3679);
#2864=DIRECTION('axis',(0.,0.,1.));
#2865=DIRECTION('refdir',(1.,0.,0.));
#2866=DIRECTION('axis',(0.,0.,1.));
#2867=DIRECTION('refdir',(1.,0.,0.));
#2868=DIRECTION('center_axis',(0.,1.,0.));
#2869=DIRECTION('ref_axis',(0.,0.,1.));
#2870=DIRECTION('',(-1.04972719197331E-16,0.515038073775726,-0.857167301383686));
#2871=DIRECTION('center_axis',(0.,1.,0.));
#2872=DIRECTION('ref_axis',(0.,0.,1.));
#2873=DIRECTION('center_axis',(0.,1.,0.));
#2874=DIRECTION('ref_axis',(0.,0.,1.));
#2875=DIRECTION('',(0.,1.,0.));
#2876=DIRECTION('center_axis',(0.,1.,0.));
#2877=DIRECTION('ref_axis',(0.,0.,1.));
#2878=DIRECTION('center_axis',(0.,1.,0.));
#2879=DIRECTION('ref_axis',(0.,0.,1.));
#2880=DIRECTION('',(-1.04972719197331E-16,0.515038073775726,-0.857167301383686));
#2881=DIRECTION('center_axis',(0.,1.,0.));
#2882=DIRECTION('ref_axis',(0.,0.,1.));
#2883=DIRECTION('center_axis',(0.,1.,0.));
#2884=DIRECTION('ref_axis',(0.,0.,1.));
#2885=DIRECTION('',(0.,1.,0.));
#2886=DIRECTION('center_axis',(0.,1.,0.));
#2887=DIRECTION('ref_axis',(0.,0.,1.));
#2888=DIRECTION('center_axis',(0.,1.,0.));
#2889=DIRECTION('ref_axis',(0.,0.,1.));
#2890=DIRECTION('',(-1.04972719197331E-16,0.515038073775726,-0.857167301383686));
#2891=DIRECTION('center_axis',(0.,1.,0.));
#2892=DIRECTION('ref_axis',(0.,0.,1.));
#2893=DIRECTION('center_axis',(0.,1.,0.));
#2894=DIRECTION('ref_axis',(0.,0.,1.));
#2895=DIRECTION('',(0.,1.,0.));
#2896=DIRECTION('center_axis',(0.,1.,0.));
#2897=DIRECTION('ref_axis',(0.,0.,1.));
#2898=DIRECTION('center_axis',(0.,1.,0.));
#2899=DIRECTION('ref_axis',(0.,0.,1.));
#2900=DIRECTION('',(-1.04972719197331E-16,0.515038073775726,-0.857167301383686));
#2901=DIRECTION('center_axis',(0.,1.,0.));
#2902=DIRECTION('ref_axis',(0.,0.,1.));
#2903=DIRECTION('center_axis',(0.,1.,0.));
#2904=DIRECTION('ref_axis',(0.,0.,1.));
#2905=DIRECTION('',(0.,1.,0.));
#2906=DIRECTION('center_axis',(0.,1.,0.));
#2907=DIRECTION('ref_axis',(0.,0.,1.));
#2908=DIRECTION('center_axis',(0.,1.,0.));
#2909=DIRECTION('ref_axis',(0.,0.,1.));
#2910=DIRECTION('center_axis',(0.,0.707106781186548,-0.707106781186548));
#2911=DIRECTION('ref_axis',(1.76988781740397E-14,0.707106781186548,0.707106781186548));
#2912=DIRECTION('center_axis',(0.,0.707106781186548,0.707106781186548));
#2913=DIRECTION('ref_axis',(7.96449517831793E-15,-0.707106781186548,0.707106781186548));
#2914=DIRECTION('',(0.,1.,0.));
#2915=DIRECTION('center_axis',(0.,1.,0.));
#2916=DIRECTION('ref_axis',(0.,0.,1.));
#2917=DIRECTION('center_axis',(0.,0.707106781186548,0.707106781186548));
#2918=DIRECTION('ref_axis',(7.96449517831793E-15,-0.707106781186548,0.707106781186548));
#2919=DIRECTION('center_axis',(0.,0.,-1.));
#2920=DIRECTION('ref_axis',(-1.,0.,0.));
#2921=DIRECTION('center_axis',(0.,0.,-1.));
#2922=DIRECTION('ref_axis',(-1.,0.,0.));
#2923=DIRECTION('',(0.,0.,-1.));
#2924=DIRECTION('center_axis',(0.,0.,1.));
#2925=DIRECTION('ref_axis',(1.,0.,0.));
#2926=DIRECTION('',(0.,0.,-1.));
#2927=DIRECTION('',(0.,0.,1.));
#2928=DIRECTION('center_axis',(0.,0.,-1.));
#2929=DIRECTION('ref_axis',(-1.,0.,0.));
#2930=DIRECTION('center_axis',(0.,0.,1.));
#2931=DIRECTION('ref_axis',(1.,0.,0.));
#2932=DIRECTION('',(0.,0.,-1.));
#2933=DIRECTION('center_axis',(8.67361737988403E-17,0.,1.));
#2934=DIRECTION('ref_axis',(1.,0.,-8.67361737988404E-17));
#2935=DIRECTION('',(0.,0.,1.));
#2936=DIRECTION('',(0.,0.,-1.));
#2937=DIRECTION('center_axis',(0.,0.,-1.));
#2938=DIRECTION('ref_axis',(-1.,0.,0.));
#2939=DIRECTION('',(0.,1.,0.));
#2940=DIRECTION('',(-1.,0.,0.));
#2941=DIRECTION('',(0.,-1.,0.));
#2942=DIRECTION('',(1.,0.,0.));
#2943=DIRECTION('center_axis',(0.,0.,-1.));
#2944=DIRECTION('ref_axis',(-1.,0.,0.));
#2945=DIRECTION('',(0.,1.,0.));
#2946=DIRECTION('',(1.,0.,0.));
#2947=DIRECTION('',(0.,-1.,0.));
#2948=DIRECTION('',(-1.,0.,0.));
#2949=DIRECTION('center_axis',(-1.,0.,0.));
#2950=DIRECTION('ref_axis',(0.,0.,1.));
#2951=DIRECTION('',(0.,0.,-1.));
#2952=DIRECTION('',(0.,0.,-1.));
#2953=DIRECTION('center_axis',(0.,-1.,0.));
#2954=DIRECTION('ref_axis',(0.,0.,-1.));
#2955=DIRECTION('',(0.,0.,-1.));
#2956=DIRECTION('center_axis',(1.,0.,0.));
#2957=DIRECTION('ref_axis',(0.,0.,-1.));
#2958=DIRECTION('',(0.,0.,-1.));
#2959=DIRECTION('center_axis',(0.,1.,0.));
#2960=DIRECTION('ref_axis',(0.,0.,1.));
#2961=DIRECTION('center_axis',(0.,0.,-1.));
#2962=DIRECTION('ref_axis',(-1.,0.,0.));
#2963=DIRECTION('',(1.,0.,0.));
#2964=DIRECTION('center_axis',(8.67361737988403E-17,0.,1.));
#2965=DIRECTION('ref_axis',(1.,0.,-8.67361737988404E-17));
#2966=DIRECTION('',(-1.,0.,8.67361737988404E-17));
#2967=DIRECTION('center_axis',(0.,1.,0.));
#2968=DIRECTION('ref_axis',(0.,0.,1.));
#2969=DIRECTION('axis',(0.,0.,1.));
#2970=DIRECTION('refdir',(1.,0.,0.));
#2971=DIRECTION('center_axis',(0.,1.,0.));
#2972=DIRECTION('ref_axis',(0.,0.,1.));
#2973=DIRECTION('center_axis',(0.,1.,0.));
#2974=DIRECTION('ref_axis',(0.,0.,1.));
#2975=DIRECTION('',(0.,1.,0.));
#2976=DIRECTION('center_axis',(0.,1.,0.));
#2977=DIRECTION('ref_axis',(0.,0.,1.));
#2978=DIRECTION('center_axis',(0.,1.,0.));
#2979=DIRECTION('ref_axis',(0.,0.,1.));
#2980=DIRECTION('center_axis',(0.,1.,0.));
#2981=DIRECTION('ref_axis',(0.,0.,1.));
#2982=DIRECTION('',(0.,-1.,0.));
#2983=DIRECTION('center_axis',(0.,1.,0.));
#2984=DIRECTION('ref_axis',(0.,0.,1.));
#2985=DIRECTION('center_axis',(0.,-1.,0.));
#2986=DIRECTION('ref_axis',(0.,0.,-1.));
#2987=DIRECTION('center_axis',(0.,-1.,0.));
#2988=DIRECTION('ref_axis',(0.,0.,-1.));
#2989=DIRECTION('',(0.,1.,0.));
#2990=DIRECTION('center_axis',(0.,-1.,0.));
#2991=DIRECTION('ref_axis',(0.,0.,-1.));
#2992=DIRECTION('center_axis',(0.,-1.,0.));
#2993=DIRECTION('ref_axis',(0.,0.,-1.));
#2994=DIRECTION('center_axis',(0.,-1.,0.));
#2995=DIRECTION('ref_axis',(0.,0.,-1.));
#2996=DIRECTION('',(0.,1.,0.));
#2997=DIRECTION('center_axis',(0.,1.,0.));
#2998=DIRECTION('ref_axis',(0.,0.,1.));
#2999=DIRECTION('center_axis',(0.,-1.,0.));
#3000=DIRECTION('ref_axis',(0.,0.,-1.));
#3001=DIRECTION('center_axis',(0.,1.,0.));
#3002=DIRECTION('ref_axis',(0.,0.,1.));
#3003=DIRECTION('center_axis',(0.,1.,0.));
#3004=DIRECTION('ref_axis',(0.,0.,1.));
#3005=DIRECTION('center_axis',(0.,1.,0.));
#3006=DIRECTION('ref_axis',(0.,0.,1.));
#3007=DIRECTION('center_axis',(0.,1.,0.));
#3008=DIRECTION('ref_axis',(0.,0.,1.));
#3009=DIRECTION('axis',(0.,0.,1.));
#3010=DIRECTION('refdir',(1.,0.,0.));
#3011=DIRECTION('center_axis',(0.,1.,0.));
#3012=DIRECTION('ref_axis',(0.,0.,1.));
#3013=DIRECTION('center_axis',(0.,-1.,0.));
#3014=DIRECTION('ref_axis',(0.,0.,-1.));
#3015=DIRECTION('',(0.,1.,0.));
#3016=DIRECTION('center_axis',(0.,-1.,0.));
#3017=DIRECTION('ref_axis',(0.,0.,-1.));
#3018=DIRECTION('center_axis',(0.,1.,0.));
#3019=DIRECTION('ref_axis',(0.,0.,1.));
#3020=DIRECTION('center_axis',(0.,-1.,0.));
#3021=DIRECTION('ref_axis',(0.,0.,-1.));
#3022=DIRECTION('',(0.,-1.,0.));
#3023=DIRECTION('center_axis',(0.,-1.,0.));
#3024=DIRECTION('ref_axis',(0.,0.,-1.));
#3025=DIRECTION('center_axis',(0.,-1.,0.));
#3026=DIRECTION('ref_axis',(0.,0.,-1.));
#3027=DIRECTION('center_axis',(0.,-1.,0.));
#3028=DIRECTION('ref_axis',(0.,0.,-1.));
#3029=DIRECTION('center_axis',(0.,-1.,0.));
#3030=DIRECTION('ref_axis',(0.,0.,-1.));
#3031=DIRECTION('axis',(0.,0.,1.));
#3032=DIRECTION('refdir',(1.,0.,0.));
#3033=DIRECTION('center_axis',(1.02811330220411E-14,-0.112954554410665,
0.993600155312935));
#3034=DIRECTION('ref_axis',(2.38360928778941E-29,0.993600155312935,0.112954554410665));
#3035=DIRECTION('center_axis',(-1.02811330220411E-14,0.112954554410665,
-0.993600155312935));
#3036=DIRECTION('ref_axis',(1.8514835708046E-30,0.993600155312935,0.112954554410665));
#3037=DIRECTION('center_axis',(1.04703450427522E-14,-0.112954554410665,
0.993600155312935));
#3038=DIRECTION('ref_axis',(-2.63248751403759E-32,-0.993600155312935,-0.112954554410665));
#3039=DIRECTION('',(-1.,0.,1.053778523158E-14));
#3040=DIRECTION('center_axis',(-1.02811330220411E-14,0.112954554410665,
-0.993600155312935));
#3041=DIRECTION('ref_axis',(1.8514835708046E-30,0.993600155312935,0.112954554410665));
#3042=DIRECTION('center_axis',(1.02744001254975E-14,-0.112954554410666,
0.993600155312935));
#3043=DIRECTION('ref_axis',(-6.45044998851022E-32,-0.993600155312935,-0.112954554410666));
#3044=DIRECTION('center_axis',(1.02811330220411E-14,-0.112954554410665,
0.993600155312935));
#3045=DIRECTION('ref_axis',(2.38360928778941E-29,0.993600155312935,0.112954554410665));
#3046=DIRECTION('center_axis',(0.,1.,0.));
#3047=DIRECTION('ref_axis',(0.,0.,1.));
#3048=DIRECTION('axis',(0.,0.,1.));
#3049=DIRECTION('refdir',(1.,0.,0.));
#3050=DIRECTION('center_axis',(0.,1.,0.));
#3051=DIRECTION('ref_axis',(0.,0.,1.));
#3052=DIRECTION('center_axis',(0.,1.,0.));
#3053=DIRECTION('ref_axis',(0.,0.,1.));
#3054=DIRECTION('',(0.,1.,0.));
#3055=DIRECTION('center_axis',(0.,-1.,0.));
#3056=DIRECTION('ref_axis',(0.,0.,-1.));
#3057=DIRECTION('center_axis',(0.,1.,0.));
#3058=DIRECTION('ref_axis',(0.,0.,1.));
#3059=DIRECTION('center_axis',(0.,1.,0.));
#3060=DIRECTION('ref_axis',(0.,0.,1.));
#3061=DIRECTION('',(0.,1.,0.));
#3062=DIRECTION('center_axis',(0.,-1.,0.));
#3063=DIRECTION('ref_axis',(0.,0.,-1.));
#3064=DIRECTION('center_axis',(0.,1.,0.));
#3065=DIRECTION('ref_axis',(0.,0.,1.));
#3066=DIRECTION('center_axis',(0.,1.,0.));
#3067=DIRECTION('ref_axis',(0.,0.,1.));
#3068=DIRECTION('',(0.,1.,0.));
#3069=DIRECTION('center_axis',(0.,-1.,0.));
#3070=DIRECTION('ref_axis',(0.,0.,-1.));
#3071=DIRECTION('center_axis',(0.,1.,0.));
#3072=DIRECTION('ref_axis',(0.,0.,1.));
#3073=DIRECTION('center_axis',(0.,1.,0.));
#3074=DIRECTION('ref_axis',(0.,0.,1.));
#3075=DIRECTION('',(0.,1.,0.));
#3076=DIRECTION('center_axis',(0.,-1.,0.));
#3077=DIRECTION('ref_axis',(0.,0.,-1.));
#3078=DIRECTION('center_axis',(0.,-1.,0.));
#3079=DIRECTION('ref_axis',(0.,0.,-1.));
#3080=DIRECTION('center_axis',(0.,1.,0.));
#3081=DIRECTION('ref_axis',(0.,0.,1.));
#3082=DIRECTION('',(0.,-1.,0.));
#3083=DIRECTION('center_axis',(0.,1.,0.));
#3084=DIRECTION('ref_axis',(0.,0.,1.));
#3085=DIRECTION('center_axis',(0.,-1.,0.));
#3086=DIRECTION('ref_axis',(0.,0.,-1.));
#3087=DIRECTION('',(0.,0.,-1.));
#3088=DIRECTION('',(1.,0.,0.));
#3089=DIRECTION('',(0.,0.,1.));
#3090=DIRECTION('',(-1.,0.,0.));
#3091=DIRECTION('center_axis',(0.,-1.,0.));
#3092=DIRECTION('ref_axis',(0.,0.,-1.));
#3093=DIRECTION('',(0.,0.,-1.));
#3094=DIRECTION('',(-1.,0.,0.));
#3095=DIRECTION('',(0.,0.,1.));
#3096=DIRECTION('',(1.,0.,0.));
#3097=DIRECTION('center_axis',(-1.,0.,0.));
#3098=DIRECTION('ref_axis',(0.,0.,1.));
#3099=DIRECTION('',(0.,-1.,0.));
#3100=DIRECTION('',(0.,-1.,0.));
#3101=DIRECTION('center_axis',(0.,0.,1.));
#3102=DIRECTION('ref_axis',(1.,0.,0.));
#3103=DIRECTION('',(0.,-1.,0.));
#3104=DIRECTION('center_axis',(1.,0.,0.));
#3105=DIRECTION('ref_axis',(0.,0.,-1.));
#3106=DIRECTION('',(0.,-1.,0.));
#3107=DIRECTION('center_axis',(0.,0.,-1.));
#3108=DIRECTION('ref_axis',(-1.,0.,0.));
#3109=DIRECTION('axis',(0.,0.,1.));
#3110=DIRECTION('refdir',(1.,0.,0.));
#3111=DIRECTION('center_axis',(0.,-1.,0.));
#3112=DIRECTION('ref_axis',(0.,0.,-1.));
#3113=DIRECTION('center_axis',(0.,1.,0.));
#3114=DIRECTION('ref_axis',(0.,0.,1.));
#3115=DIRECTION('',(0.,-1.,0.));
#3116=DIRECTION('center_axis',(0.,1.,0.));
#3117=DIRECTION('ref_axis',(0.,0.,1.));
#3118=DIRECTION('center_axis',(0.,-1.,0.));
#3119=DIRECTION('ref_axis',(0.,0.,-1.));
#3120=DIRECTION('center_axis',(0.,1.,0.));
#3121=DIRECTION('ref_axis',(0.,0.,1.));
#3122=DIRECTION('',(0.,-1.,0.));
#3123=DIRECTION('center_axis',(0.,1.,0.));
#3124=DIRECTION('ref_axis',(0.,0.,1.));
#3125=DIRECTION('',(0.,-1.,0.));
#3126=DIRECTION('center_axis',(0.,1.,0.));
#3127=DIRECTION('ref_axis',(0.,0.,1.));
#3128=DIRECTION('center_axis',(0.,1.,0.));
#3129=DIRECTION('ref_axis',(0.,0.,1.));
#3130=DIRECTION('',(3.46944695195362E-16,0.,1.));
#3131=DIRECTION('',(-3.46944695195361E-16,0.,-1.));
#3132=DIRECTION('center_axis',(0.,-1.,0.));
#3133=DIRECTION('ref_axis',(1.22464679914735E-16,0.,1.));
#3134=DIRECTION('',(0.,-1.,0.));
#3135=DIRECTION('center_axis',(0.,1.,0.));
#3136=DIRECTION('ref_axis',(0.,0.,1.));
#3137=DIRECTION('',(0.,-1.,0.));
#3138=DIRECTION('center_axis',(-1.,0.,3.46944695195361E-16));
#3139=DIRECTION('ref_axis',(3.46944695195361E-16,0.,1.));
#3140=DIRECTION('',(-3.46944695195361E-16,0.,-1.));
#3141=DIRECTION('center_axis',(1.,0.,-3.46944695195362E-16));
#3142=DIRECTION('ref_axis',(-3.46944695195362E-16,0.,-1.));
#3143=DIRECTION('',(3.46944695195361E-16,0.,1.));
#3144=DIRECTION('center_axis',(0.,1.,0.));
#3145=DIRECTION('ref_axis',(0.,0.,1.));
#3146=DIRECTION('center_axis',(0.,1.,0.));
#3147=DIRECTION('ref_axis',(0.,0.,1.));
#3148=DIRECTION('axis',(0.,0.,1.));
#3149=DIRECTION('refdir',(1.,0.,0.));
#3150=DIRECTION('center_axis',(0.,-1.,0.));
#3151=DIRECTION('ref_axis',(1.22464679914735E-16,0.,1.));
#3152=DIRECTION('center_axis',(0.,0.,1.));
#3153=DIRECTION('ref_axis',(1.,0.,0.));
#3154=DIRECTION('center_axis',(0.,1.,0.));
#3155=DIRECTION('ref_axis',(1.22464679914735E-16,0.,1.));
#3156=DIRECTION('center_axis',(-4.91504984860095E-16,0.,-1.));
#3157=DIRECTION('ref_axis',(-1.,0.,4.91504984860095E-16));
#3158=DIRECTION('center_axis',(0.,-1.,0.));
#3159=DIRECTION('ref_axis',(0.,0.,-1.));
#3160=DIRECTION('center_axis',(-3.37307342551046E-16,0.,-1.));
#3161=DIRECTION('ref_axis',(-1.,0.,3.37307342551046E-16));
#3162=DIRECTION('center_axis',(0.,1.,0.));
#3163=DIRECTION('ref_axis',(0.,0.,-1.));
#3164=DIRECTION('center_axis',(0.,0.,1.));
#3165=DIRECTION('ref_axis',(1.,0.,0.));
#3166=DIRECTION('center_axis',(-3.46944695195361E-16,0.,-1.));
#3167=DIRECTION('ref_axis',(-1.,0.,3.46944695195361E-16));
#3168=DIRECTION('',(3.46944695195361E-16,0.,1.));
#3169=DIRECTION('center_axis',(3.46944695195361E-16,0.,1.));
#3170=DIRECTION('ref_axis',(1.,0.,-3.46944695195361E-16));
#3171=DIRECTION('',(-3.46944695195361E-16,0.,-1.));
#3172=DIRECTION('center_axis',(0.,-1.,0.));
#3173=DIRECTION('ref_axis',(1.22464679914735E-16,0.,1.));
#3174=DIRECTION('center_axis',(0.,0.,1.));
#3175=DIRECTION('ref_axis',(1.,0.,0.));
#3176=DIRECTION('center_axis',(0.,1.,0.));
#3177=DIRECTION('ref_axis',(1.22464679914735E-16,0.,1.));
#3178=DIRECTION('center_axis',(-4.91504984860095E-16,0.,-1.));
#3179=DIRECTION('ref_axis',(-1.,0.,4.91504984860095E-16));
#3180=DIRECTION('center_axis',(0.,-1.,0.));
#3181=DIRECTION('ref_axis',(0.,0.,-1.));
#3182=DIRECTION('center_axis',(-3.37307342551046E-16,0.,-1.));
#3183=DIRECTION('ref_axis',(-1.,0.,3.37307342551046E-16));
#3184=DIRECTION('center_axis',(0.,1.,0.));
#3185=DIRECTION('ref_axis',(0.,0.,-1.));
#3186=DIRECTION('center_axis',(0.,0.,1.));
#3187=DIRECTION('ref_axis',(1.,0.,0.));
#3188=DIRECTION('center_axis',(-3.46944695195361E-16,0.,-1.));
#3189=DIRECTION('ref_axis',(-1.,0.,3.46944695195361E-16));
#3190=DIRECTION('',(3.46944695195361E-16,0.,1.));
#3191=DIRECTION('center_axis',(3.46944695195361E-16,0.,1.));
#3192=DIRECTION('ref_axis',(1.,0.,-3.46944695195361E-16));
#3193=DIRECTION('',(-3.46944695195361E-16,0.,-1.));
#3194=DIRECTION('center_axis',(0.,-1.,0.));
#3195=DIRECTION('ref_axis',(1.22464679914735E-16,0.,1.));
#3196=DIRECTION('center_axis',(0.,0.,1.));
#3197=DIRECTION('ref_axis',(1.,0.,0.));
#3198=DIRECTION('center_axis',(0.,1.,0.));
#3199=DIRECTION('ref_axis',(1.22464679914735E-16,0.,1.));
#3200=DIRECTION('center_axis',(-4.91504984860095E-16,0.,-1.));
#3201=DIRECTION('ref_axis',(-1.,0.,4.91504984860095E-16));
#3202=DIRECTION('center_axis',(0.,-1.,0.));
#3203=DIRECTION('ref_axis',(0.,0.,-1.));
#3204=DIRECTION('center_axis',(-3.37307342551046E-16,0.,-1.));
#3205=DIRECTION('ref_axis',(-1.,0.,3.37307342551046E-16));
#3206=DIRECTION('center_axis',(0.,1.,0.));
#3207=DIRECTION('ref_axis',(0.,0.,-1.));
#3208=DIRECTION('center_axis',(0.,0.,1.));
#3209=DIRECTION('ref_axis',(1.,0.,0.));
#3210=DIRECTION('center_axis',(-3.46944695195361E-16,0.,-1.));
#3211=DIRECTION('ref_axis',(-1.,0.,3.46944695195361E-16));
#3212=DIRECTION('',(3.46944695195361E-16,0.,1.));
#3213=DIRECTION('center_axis',(3.46944695195361E-16,0.,1.));
#3214=DIRECTION('ref_axis',(1.,0.,-3.46944695195361E-16));
#3215=DIRECTION('',(-3.46944695195361E-16,0.,-1.));
#3216=DIRECTION('center_axis',(0.,-1.,0.));
#3217=DIRECTION('ref_axis',(1.22464679914735E-16,0.,1.));
#3218=DIRECTION('center_axis',(0.,0.,1.));
#3219=DIRECTION('ref_axis',(1.,0.,0.));
#3220=DIRECTION('center_axis',(0.,1.,0.));
#3221=DIRECTION('ref_axis',(1.22464679914735E-16,0.,1.));
#3222=DIRECTION('center_axis',(-4.91504984860095E-16,0.,-1.));
#3223=DIRECTION('ref_axis',(-1.,0.,4.91504984860095E-16));
#3224=DIRECTION('center_axis',(0.,-1.,0.));
#3225=DIRECTION('ref_axis',(0.,0.,-1.));
#3226=DIRECTION('center_axis',(-3.37307342551046E-16,0.,-1.));
#3227=DIRECTION('ref_axis',(-1.,0.,3.37307342551046E-16));
#3228=DIRECTION('center_axis',(0.,1.,0.));
#3229=DIRECTION('ref_axis',(0.,0.,-1.));
#3230=DIRECTION('center_axis',(0.,0.,1.));
#3231=DIRECTION('ref_axis',(1.,0.,0.));
#3232=DIRECTION('center_axis',(-3.46944695195361E-16,0.,-1.));
#3233=DIRECTION('ref_axis',(-1.,0.,3.46944695195361E-16));
#3234=DIRECTION('',(3.46944695195361E-16,0.,1.));
#3235=DIRECTION('center_axis',(3.46944695195361E-16,0.,1.));
#3236=DIRECTION('ref_axis',(1.,0.,-3.46944695195361E-16));
#3237=DIRECTION('',(-3.46944695195361E-16,0.,-1.));
#3238=DIRECTION('center_axis',(0.,-1.,0.));
#3239=DIRECTION('ref_axis',(1.22464679914735E-16,0.,1.));
#3240=DIRECTION('center_axis',(0.,0.,1.));
#3241=DIRECTION('ref_axis',(1.,0.,0.));
#3242=DIRECTION('center_axis',(0.,1.,0.));
#3243=DIRECTION('ref_axis',(1.22464679914735E-16,0.,1.));
#3244=DIRECTION('center_axis',(-4.91504984860095E-16,0.,-1.));
#3245=DIRECTION('ref_axis',(-1.,0.,4.91504984860095E-16));
#3246=DIRECTION('center_axis',(0.,-1.,0.));
#3247=DIRECTION('ref_axis',(0.,0.,-1.));
#3248=DIRECTION('center_axis',(-3.37307342551046E-16,0.,-1.));
#3249=DIRECTION('ref_axis',(-1.,0.,3.37307342551046E-16));
#3250=DIRECTION('center_axis',(0.,1.,0.));
#3251=DIRECTION('ref_axis',(0.,0.,-1.));
#3252=DIRECTION('center_axis',(0.,0.,1.));
#3253=DIRECTION('ref_axis',(1.,0.,0.));
#3254=DIRECTION('center_axis',(-3.46944695195361E-16,0.,-1.));
#3255=DIRECTION('ref_axis',(-1.,0.,3.46944695195361E-16));
#3256=DIRECTION('',(3.46944695195361E-16,0.,1.));
#3257=DIRECTION('center_axis',(3.46944695195361E-16,0.,1.));
#3258=DIRECTION('ref_axis',(1.,0.,-3.46944695195361E-16));
#3259=DIRECTION('',(-3.46944695195361E-16,0.,-1.));
#3260=DIRECTION('center_axis',(0.,-1.,0.));
#3261=DIRECTION('ref_axis',(1.22464679914735E-16,0.,1.));
#3262=DIRECTION('center_axis',(0.,0.,1.));
#3263=DIRECTION('ref_axis',(1.,0.,0.));
#3264=DIRECTION('center_axis',(0.,1.,0.));
#3265=DIRECTION('ref_axis',(1.22464679914735E-16,0.,1.));
#3266=DIRECTION('center_axis',(-4.91504984860095E-16,0.,-1.));
#3267=DIRECTION('ref_axis',(-1.,0.,4.91504984860095E-16));
#3268=DIRECTION('center_axis',(0.,-1.,0.));
#3269=DIRECTION('ref_axis',(0.,0.,-1.));
#3270=DIRECTION('center_axis',(-3.37307342551046E-16,0.,-1.));
#3271=DIRECTION('ref_axis',(-1.,0.,3.37307342551046E-16));
#3272=DIRECTION('center_axis',(0.,1.,0.));
#3273=DIRECTION('ref_axis',(0.,0.,-1.));
#3274=DIRECTION('center_axis',(0.,0.,1.));
#3275=DIRECTION('ref_axis',(1.,0.,0.));
#3276=DIRECTION('center_axis',(-3.46944695195361E-16,0.,-1.));
#3277=DIRECTION('ref_axis',(-1.,0.,3.46944695195361E-16));
#3278=DIRECTION('',(3.46944695195361E-16,0.,1.));
#3279=DIRECTION('center_axis',(3.46944695195361E-16,0.,1.));
#3280=DIRECTION('ref_axis',(1.,0.,-3.46944695195361E-16));
#3281=DIRECTION('',(-3.46944695195361E-16,0.,-1.));
#3282=DIRECTION('center_axis',(0.,-1.,0.));
#3283=DIRECTION('ref_axis',(1.22464679914735E-16,0.,1.));
#3284=DIRECTION('center_axis',(0.,0.,1.));
#3285=DIRECTION('ref_axis',(1.,0.,0.));
#3286=DIRECTION('center_axis',(0.,1.,0.));
#3287=DIRECTION('ref_axis',(1.22464679914735E-16,0.,1.));
#3288=DIRECTION('center_axis',(-4.91504984860095E-16,0.,-1.));
#3289=DIRECTION('ref_axis',(-1.,0.,4.91504984860095E-16));
#3290=DIRECTION('center_axis',(0.,-1.,0.));
#3291=DIRECTION('ref_axis',(0.,0.,-1.));
#3292=DIRECTION('center_axis',(-3.37307342551046E-16,0.,-1.));
#3293=DIRECTION('ref_axis',(-1.,0.,3.37307342551046E-16));
#3294=DIRECTION('center_axis',(0.,1.,0.));
#3295=DIRECTION('ref_axis',(0.,0.,-1.));
#3296=DIRECTION('center_axis',(0.,0.,1.));
#3297=DIRECTION('ref_axis',(1.,0.,0.));
#3298=DIRECTION('center_axis',(-3.46944695195361E-16,0.,-1.));
#3299=DIRECTION('ref_axis',(-1.,0.,3.46944695195361E-16));
#3300=DIRECTION('',(3.46944695195361E-16,0.,1.));
#3301=DIRECTION('center_axis',(3.46944695195361E-16,0.,1.));
#3302=DIRECTION('ref_axis',(1.,0.,-3.46944695195361E-16));
#3303=DIRECTION('',(-3.46944695195361E-16,0.,-1.));
#3304=DIRECTION('center_axis',(0.,-1.,0.));
#3305=DIRECTION('ref_axis',(1.22464679914735E-16,0.,1.));
#3306=DIRECTION('center_axis',(0.,0.,1.));
#3307=DIRECTION('ref_axis',(1.,0.,0.));
#3308=DIRECTION('center_axis',(0.,1.,0.));
#3309=DIRECTION('ref_axis',(1.22464679914735E-16,0.,1.));
#3310=DIRECTION('center_axis',(-4.91504984860095E-16,0.,-1.));
#3311=DIRECTION('ref_axis',(-1.,0.,4.91504984860095E-16));
#3312=DIRECTION('center_axis',(0.,-1.,0.));
#3313=DIRECTION('ref_axis',(0.,0.,-1.));
#3314=DIRECTION('center_axis',(-3.37307342551046E-16,0.,-1.));
#3315=DIRECTION('ref_axis',(-1.,0.,3.37307342551046E-16));
#3316=DIRECTION('center_axis',(0.,1.,0.));
#3317=DIRECTION('ref_axis',(0.,0.,-1.));
#3318=DIRECTION('center_axis',(0.,0.,1.));
#3319=DIRECTION('ref_axis',(1.,0.,0.));
#3320=DIRECTION('center_axis',(-3.46944695195361E-16,0.,-1.));
#3321=DIRECTION('ref_axis',(-1.,0.,3.46944695195361E-16));
#3322=DIRECTION('',(3.46944695195361E-16,0.,1.));
#3323=DIRECTION('center_axis',(3.46944695195361E-16,0.,1.));
#3324=DIRECTION('ref_axis',(1.,0.,-3.46944695195361E-16));
#3325=DIRECTION('',(-3.46944695195361E-16,0.,-1.));
#3326=DIRECTION('center_axis',(0.,-1.,0.));
#3327=DIRECTION('ref_axis',(1.22464679914735E-16,0.,1.));
#3328=DIRECTION('center_axis',(0.,0.,1.));
#3329=DIRECTION('ref_axis',(1.,0.,0.));
#3330=DIRECTION('center_axis',(0.,1.,0.));
#3331=DIRECTION('ref_axis',(1.22464679914735E-16,0.,1.));
#3332=DIRECTION('center_axis',(-4.91504984860095E-16,0.,-1.));
#3333=DIRECTION('ref_axis',(-1.,0.,4.91504984860095E-16));
#3334=DIRECTION('center_axis',(0.,-1.,0.));
#3335=DIRECTION('ref_axis',(0.,0.,-1.));
#3336=DIRECTION('center_axis',(-3.37307342551046E-16,0.,-1.));
#3337=DIRECTION('ref_axis',(-1.,0.,3.37307342551046E-16));
#3338=DIRECTION('center_axis',(0.,1.,0.));
#3339=DIRECTION('ref_axis',(0.,0.,-1.));
#3340=DIRECTION('center_axis',(0.,0.,1.));
#3341=DIRECTION('ref_axis',(1.,0.,0.));
#3342=DIRECTION('center_axis',(-3.46944695195361E-16,0.,-1.));
#3343=DIRECTION('ref_axis',(-1.,0.,3.46944695195361E-16));
#3344=DIRECTION('',(3.46944695195361E-16,0.,1.));
#3345=DIRECTION('center_axis',(3.46944695195361E-16,0.,1.));
#3346=DIRECTION('ref_axis',(1.,0.,-3.46944695195361E-16));
#3347=DIRECTION('',(-3.46944695195361E-16,0.,-1.));
#3348=DIRECTION('center_axis',(0.,-1.,0.));
#3349=DIRECTION('ref_axis',(1.22464679914735E-16,0.,1.));
#3350=DIRECTION('center_axis',(0.,0.,1.));
#3351=DIRECTION('ref_axis',(1.,0.,0.));
#3352=DIRECTION('center_axis',(0.,1.,0.));
#3353=DIRECTION('ref_axis',(1.22464679914735E-16,0.,1.));
#3354=DIRECTION('center_axis',(-4.91504984860095E-16,0.,-1.));
#3355=DIRECTION('ref_axis',(-1.,0.,4.91504984860095E-16));
#3356=DIRECTION('center_axis',(0.,-1.,0.));
#3357=DIRECTION('ref_axis',(0.,0.,-1.));
#3358=DIRECTION('center_axis',(-3.37307342551046E-16,0.,-1.));
#3359=DIRECTION('ref_axis',(-1.,0.,3.37307342551046E-16));
#3360=DIRECTION('center_axis',(0.,1.,0.));
#3361=DIRECTION('ref_axis',(0.,0.,-1.));
#3362=DIRECTION('center_axis',(0.,0.,1.));
#3363=DIRECTION('ref_axis',(1.,0.,0.));
#3364=DIRECTION('center_axis',(-3.46944695195361E-16,0.,-1.));
#3365=DIRECTION('ref_axis',(-1.,0.,3.46944695195361E-16));
#3366=DIRECTION('',(3.46944695195361E-16,0.,1.));
#3367=DIRECTION('center_axis',(3.46944695195361E-16,0.,1.));
#3368=DIRECTION('ref_axis',(1.,0.,-3.46944695195361E-16));
#3369=DIRECTION('',(-3.46944695195361E-16,0.,-1.));
#3370=DIRECTION('center_axis',(0.,-1.,0.));
#3371=DIRECTION('ref_axis',(1.22464679914735E-16,0.,1.));
#3372=DIRECTION('center_axis',(0.,0.,1.));
#3373=DIRECTION('ref_axis',(1.,0.,0.));
#3374=DIRECTION('center_axis',(0.,1.,0.));
#3375=DIRECTION('ref_axis',(1.22464679914735E-16,0.,1.));
#3376=DIRECTION('center_axis',(-4.91504984860095E-16,0.,-1.));
#3377=DIRECTION('ref_axis',(-1.,0.,4.91504984860095E-16));
#3378=DIRECTION('center_axis',(0.,-1.,0.));
#3379=DIRECTION('ref_axis',(0.,0.,-1.));
#3380=DIRECTION('center_axis',(-3.37307342551046E-16,0.,-1.));
#3381=DIRECTION('ref_axis',(-1.,0.,3.37307342551046E-16));
#3382=DIRECTION('center_axis',(0.,1.,0.));
#3383=DIRECTION('ref_axis',(0.,0.,-1.));
#3384=DIRECTION('center_axis',(0.,0.,1.));
#3385=DIRECTION('ref_axis',(1.,0.,0.));
#3386=DIRECTION('center_axis',(-3.46944695195361E-16,0.,-1.));
#3387=DIRECTION('ref_axis',(-1.,0.,3.46944695195361E-16));
#3388=DIRECTION('',(3.46944695195361E-16,0.,1.));
#3389=DIRECTION('center_axis',(3.46944695195361E-16,0.,1.));
#3390=DIRECTION('ref_axis',(1.,0.,-3.46944695195361E-16));
#3391=DIRECTION('',(-3.46944695195361E-16,0.,-1.));
#3392=DIRECTION('center_axis',(0.,-1.,0.));
#3393=DIRECTION('ref_axis',(1.22464679914735E-16,0.,1.));
#3394=DIRECTION('center_axis',(0.,0.,1.));
#3395=DIRECTION('ref_axis',(1.,0.,0.));
#3396=DIRECTION('center_axis',(0.,1.,0.));
#3397=DIRECTION('ref_axis',(1.22464679914735E-16,0.,1.));
#3398=DIRECTION('center_axis',(-4.91504984860095E-16,0.,-1.));
#3399=DIRECTION('ref_axis',(-1.,0.,4.91504984860095E-16));
#3400=DIRECTION('center_axis',(0.,-1.,0.));
#3401=DIRECTION('ref_axis',(0.,0.,-1.));
#3402=DIRECTION('center_axis',(-3.37307342551046E-16,0.,-1.));
#3403=DIRECTION('ref_axis',(-1.,0.,3.37307342551046E-16));
#3404=DIRECTION('center_axis',(0.,1.,0.));
#3405=DIRECTION('ref_axis',(0.,0.,-1.));
#3406=DIRECTION('center_axis',(0.,0.,1.));
#3407=DIRECTION('ref_axis',(1.,0.,0.));
#3408=DIRECTION('center_axis',(-3.46944695195361E-16,0.,-1.));
#3409=DIRECTION('ref_axis',(-1.,0.,3.46944695195361E-16));
#3410=DIRECTION('',(3.46944695195361E-16,0.,1.));
#3411=DIRECTION('center_axis',(3.46944695195361E-16,0.,1.));
#3412=DIRECTION('ref_axis',(1.,0.,-3.46944695195361E-16));
#3413=DIRECTION('',(-3.46944695195361E-16,0.,-1.));
#3414=DIRECTION('center_axis',(0.,-1.,0.));
#3415=DIRECTION('ref_axis',(1.22464679914735E-16,0.,1.));
#3416=DIRECTION('center_axis',(0.,0.,1.));
#3417=DIRECTION('ref_axis',(1.,0.,0.));
#3418=DIRECTION('center_axis',(0.,1.,0.));
#3419=DIRECTION('ref_axis',(1.22464679914735E-16,0.,1.));
#3420=DIRECTION('center_axis',(-4.91504984860095E-16,0.,-1.));
#3421=DIRECTION('ref_axis',(-1.,0.,4.91504984860095E-16));
#3422=DIRECTION('center_axis',(0.,-1.,0.));
#3423=DIRECTION('ref_axis',(0.,0.,-1.));
#3424=DIRECTION('center_axis',(-3.37307342551046E-16,0.,-1.));
#3425=DIRECTION('ref_axis',(-1.,0.,3.37307342551046E-16));
#3426=DIRECTION('center_axis',(0.,1.,0.));
#3427=DIRECTION('ref_axis',(0.,0.,-1.));
#3428=DIRECTION('center_axis',(0.,0.,1.));
#3429=DIRECTION('ref_axis',(1.,0.,0.));
#3430=DIRECTION('center_axis',(-3.46944695195361E-16,0.,-1.));
#3431=DIRECTION('ref_axis',(-1.,0.,3.46944695195361E-16));
#3432=DIRECTION('',(3.46944695195361E-16,0.,1.));
#3433=DIRECTION('center_axis',(3.46944695195361E-16,0.,1.));
#3434=DIRECTION('ref_axis',(1.,0.,-3.46944695195361E-16));
#3435=DIRECTION('',(-3.46944695195361E-16,0.,-1.));
#3436=DIRECTION('axis',(0.,0.,1.));
#3437=DIRECTION('refdir',(1.,0.,0.));
#3438=DIRECTION('center_axis',(0.,1.,0.));
#3439=DIRECTION('ref_axis',(0.,0.,1.));
#3440=DIRECTION('center_axis',(0.,-1.,0.));
#3441=DIRECTION('ref_axis',(0.,0.,-1.));
#3442=DIRECTION('center_axis',(-1.,0.,0.));
#3443=DIRECTION('ref_axis',(0.,0.,-1.));
#3444=DIRECTION('center_axis',(0.,1.,0.));
#3445=DIRECTION('ref_axis',(0.,0.,1.));
#3446=DIRECTION('center_axis',(0.,1.,0.));
#3447=DIRECTION('ref_axis',(0.,0.,1.));
#3448=DIRECTION('center_axis',(0.,-1.,0.));
#3449=DIRECTION('ref_axis',(0.,0.,-1.));
#3450=DIRECTION('center_axis',(-1.,0.,0.));
#3451=DIRECTION('ref_axis',(0.,0.,-1.));
#3452=DIRECTION('center_axis',(0.,1.,0.));
#3453=DIRECTION('ref_axis',(0.,0.,1.));
#3454=DIRECTION('center_axis',(0.,1.,0.));
#3455=DIRECTION('ref_axis',(0.,0.,1.));
#3456=DIRECTION('center_axis',(0.,-1.,0.));
#3457=DIRECTION('ref_axis',(0.,0.,-1.));
#3458=DIRECTION('center_axis',(-1.,0.,0.));
#3459=DIRECTION('ref_axis',(0.,0.,-1.));
#3460=DIRECTION('center_axis',(0.,1.,0.));
#3461=DIRECTION('ref_axis',(0.,0.,1.));
#3462=DIRECTION('center_axis',(0.,1.,0.));
#3463=DIRECTION('ref_axis',(0.,0.,1.));
#3464=DIRECTION('center_axis',(0.,-1.,0.));
#3465=DIRECTION('ref_axis',(0.,0.,-1.));
#3466=DIRECTION('center_axis',(-1.,0.,0.));
#3467=DIRECTION('ref_axis',(0.,0.,-1.));
#3468=DIRECTION('center_axis',(0.,1.,0.));
#3469=DIRECTION('ref_axis',(0.,0.,1.));
#3470=DIRECTION('center_axis',(0.,1.,0.));
#3471=DIRECTION('ref_axis',(0.,0.,1.));
#3472=DIRECTION('center_axis',(0.,1.,0.));
#3473=DIRECTION('ref_axis',(0.,0.,1.));
#3474=DIRECTION('',(0.,1.,0.));
#3475=DIRECTION('center_axis',(0.,1.,0.));
#3476=DIRECTION('ref_axis',(0.,0.,1.));
#3477=DIRECTION('center_axis',(0.,1.,0.));
#3478=DIRECTION('ref_axis',(0.,0.,1.));
#3479=DIRECTION('',(0.,1.,0.));
#3480=DIRECTION('center_axis',(0.,1.,0.));
#3481=DIRECTION('ref_axis',(0.,0.,1.));
#3482=DIRECTION('center_axis',(0.,1.,0.));
#3483=DIRECTION('ref_axis',(0.,0.,1.));
#3484=DIRECTION('',(0.,1.,0.));
#3485=DIRECTION('center_axis',(0.,1.,0.));
#3486=DIRECTION('ref_axis',(0.,0.,1.));
#3487=DIRECTION('center_axis',(0.,1.,0.));
#3488=DIRECTION('ref_axis',(0.,0.,1.));
#3489=DIRECTION('',(0.,1.,0.));
#3490=DIRECTION('center_axis',(0.,0.,1.));
#3491=DIRECTION('ref_axis',(1.,0.,0.));
#3492=DIRECTION('',(1.,0.,0.));
#3493=DIRECTION('',(0.,-1.,0.));
#3494=DIRECTION('',(-1.,0.,0.));
#3495=DIRECTION('',(0.,-1.,0.));
#3496=DIRECTION('center_axis',(0.,0.,-1.));
#3497=DIRECTION('ref_axis',(-1.,0.,0.));
#3498=DIRECTION('',(-1.,0.,0.));
#3499=DIRECTION('',(0.,-1.,0.));
#3500=DIRECTION('',(1.,0.,0.));
#3501=DIRECTION('',(0.,-1.,0.));
#3502=DIRECTION('center_axis',(0.,1.,0.));
#3503=DIRECTION('ref_axis',(0.,0.,1.));
#3504=DIRECTION('',(0.,0.,-1.));
#3505=DIRECTION('',(1.,0.,0.));
#3506=DIRECTION('',(0.,0.,1.));
#3507=DIRECTION('',(-1.,0.,0.));
#3508=DIRECTION('',(0.,0.,-1.));
#3509=DIRECTION('',(-1.,0.,0.));
#3510=DIRECTION('',(0.,0.,1.));
#3511=DIRECTION('',(1.,0.,0.));
#3512=DIRECTION('center_axis',(-1.,0.,0.));
#3513=DIRECTION('ref_axis',(0.,0.,1.));
#3514=DIRECTION('',(0.,-1.,0.));
#3515=DIRECTION('',(0.,0.,-1.));
#3516=DIRECTION('',(0.,0.,-1.));
#3517=DIRECTION('',(0.,0.,-1.));
#3518=DIRECTION('',(0.,-1.,0.));
#3519=DIRECTION('center_axis',(1.,0.,0.));
#3520=DIRECTION('ref_axis',(0.,0.,-1.));
#3521=DIRECTION('',(0.,-1.,0.));
#3522=DIRECTION('',(0.,0.,1.));
#3523=DIRECTION('',(0.,0.,1.));
#3524=DIRECTION('',(0.,0.,1.));
#3525=DIRECTION('',(0.,-1.,0.));
#3526=DIRECTION('center_axis',(-1.,0.,0.));
#3527=DIRECTION('ref_axis',(0.,0.,1.));
#3528=DIRECTION('',(0.,-1.,0.));
#3529=DIRECTION('',(0.,0.,-1.));
#3530=DIRECTION('',(0.,-1.,0.));
#3531=DIRECTION('center_axis',(0.,0.,1.));
#3532=DIRECTION('ref_axis',(1.,0.,0.));
#3533=DIRECTION('',(-1.,0.,0.));
#3534=DIRECTION('',(0.,-1.,0.));
#3535=DIRECTION('center_axis',(1.,0.,0.));
#3536=DIRECTION('ref_axis',(0.,0.,-1.));
#3537=DIRECTION('',(0.,0.,1.));
#3538=DIRECTION('',(0.,-1.,0.));
#3539=DIRECTION('center_axis',(0.,0.,-1.));
#3540=DIRECTION('ref_axis',(-1.,0.,0.));
#3541=DIRECTION('',(1.,0.,0.));
#3542=DIRECTION('center_axis',(0.,-1.,0.));
#3543=DIRECTION('ref_axis',(0.,0.,-1.));
#3544=DIRECTION('center_axis',(0.,-1.,0.));
#3545=DIRECTION('ref_axis',(0.,0.,-1.));
#3546=DIRECTION('center_axis',(0.,0.,-1.));
#3547=DIRECTION('ref_axis',(-1.,0.,0.));
#3548=DIRECTION('',(1.,0.,0.));
#3549=DIRECTION('center_axis',(0.,-1.,0.));
#3550=DIRECTION('ref_axis',(0.,0.,-1.));
#3551=DIRECTION('center_axis',(0.,0.,1.));
#3552=DIRECTION('ref_axis',(1.,0.,0.));
#3553=DIRECTION('',(-1.,0.,0.));
#3554=DIRECTION('center_axis',(0.,-1.,0.));
#3555=DIRECTION('ref_axis',(0.,0.,-1.));
#3556=DIRECTION('axis',(0.,0.,1.));
#3557=DIRECTION('refdir',(1.,0.,0.));
#3558=DIRECTION('center_axis',(-1.,0.,0.));
#3559=DIRECTION('ref_axis',(0.,0.,1.));
#3560=DIRECTION('',(-0.500000000000004,-1.0605752387249E-16,-0.866025403784436));
#3561=DIRECTION('center_axis',(-1.,0.,0.));
#3562=DIRECTION('ref_axis',(0.,0.,1.));
#3563=DIRECTION('center_axis',(-1.,0.,0.));
#3564=DIRECTION('ref_axis',(0.,0.,1.));
#3565=DIRECTION('center_axis',(-1.,0.,0.));
#3566=DIRECTION('ref_axis',(0.,0.,1.));
#3567=DIRECTION('center_axis',(-1.,0.,0.));
#3568=DIRECTION('ref_axis',(0.,0.,1.));
#3569=DIRECTION('center_axis',(-1.,0.,0.));
#3570=DIRECTION('ref_axis',(0.,0.,1.));
#3571=DIRECTION('center_axis',(-1.,0.,0.));
#3572=DIRECTION('ref_axis',(0.,0.,1.));
#3573=DIRECTION('center_axis',(-1.,0.,0.));
#3574=DIRECTION('ref_axis',(0.,0.,1.));
#3575=DIRECTION('center_axis',(-1.,0.,0.));
#3576=DIRECTION('ref_axis',(0.,0.,1.));
#3577=DIRECTION('center_axis',(0.,1.,-1.22464679914735E-16));
#3578=DIRECTION('ref_axis',(0.,-1.22464679914735E-16,-1.));
#3579=DIRECTION('center_axis',(1.,0.,0.));
#3580=DIRECTION('ref_axis',(0.,0.,1.));
#3581=DIRECTION('center_axis',(-1.,0.,0.));
#3582=DIRECTION('ref_axis',(0.,0.,1.));
#3583=DIRECTION('center_axis',(-1.,0.,0.));
#3584=DIRECTION('ref_axis',(0.,0.,1.));
#3585=DIRECTION('',(0.707106781186549,8.65956056235492E-17,0.707106781186547));
#3586=DIRECTION('center_axis',(-1.,0.,0.));
#3587=DIRECTION('ref_axis',(0.,0.,1.));
#3588=DIRECTION('center_axis',(-1.,0.,0.));
#3589=DIRECTION('ref_axis',(0.,0.,1.));
#3590=DIRECTION('',(1.,0.,0.));
#3591=DIRECTION('center_axis',(-1.,0.,0.));
#3592=DIRECTION('ref_axis',(0.,0.,1.));
#3593=DIRECTION('center_axis',(-1.,0.,0.));
#3594=DIRECTION('ref_axis',(0.,0.,1.));
#3595=DIRECTION('',(1.,0.,0.));
#3596=DIRECTION('center_axis',(-1.,0.,0.));
#3597=DIRECTION('ref_axis',(0.,0.,1.));
#3598=DIRECTION('center_axis',(0.,6.12323399573677E-17,-1.));
#3599=DIRECTION('ref_axis',(0.,1.,0.));
#3600=DIRECTION('center_axis',(-1.,0.,0.));
#3601=DIRECTION('ref_axis',(0.,0.,1.));
#3602=DIRECTION('center_axis',(-1.,0.,0.));
#3603=DIRECTION('ref_axis',(0.,0.,1.));
#3604=DIRECTION('',(0.,-1.,1.50231459873716E-16));
#3605=DIRECTION('',(0.,-0.5,-0.866025403784438));
#3606=DIRECTION('',(0.,0.5,-0.866025403784438));
#3607=DIRECTION('',(0.,1.,0.));
#3608=DIRECTION('',(0.,0.5,0.866025403784439));
#3609=DIRECTION('',(0.,-0.5,0.866025403784438));
#3610=DIRECTION('center_axis',(-1.,0.,0.));
#3611=DIRECTION('ref_axis',(0.,0.,1.));
#3612=DIRECTION('center_axis',(-1.,0.,0.));
#3613=DIRECTION('ref_axis',(0.,0.,1.));
#3614=DIRECTION('center_axis',(0.,0.866025403784439,-0.5));
#3615=DIRECTION('ref_axis',(0.,0.5,0.866025403784439));
#3616=DIRECTION('',(0.,-0.5,-0.866025403784438));
#3617=DIRECTION('',(0.,-0.5,-0.866025403784438));
#3618=DIRECTION('',(-1.,0.,0.));
#3619=DIRECTION('',(-1.,0.,0.));
#3620=DIRECTION('center_axis',(0.,0.866025403784439,0.5));
#3621=DIRECTION('ref_axis',(0.,-0.5,0.866025403784439));
#3622=DIRECTION('',(0.,0.5,-0.866025403784438));
#3623=DIRECTION('',(0.,0.5,-0.866025403784438));
#3624=DIRECTION('',(-1.,0.,0.));
#3625=DIRECTION('center_axis',(0.,0.,1.));
#3626=DIRECTION('ref_axis',(1.,0.,0.));
#3627=DIRECTION('',(0.,1.,0.));
#3628=DIRECTION('',(0.,1.,0.));
#3629=DIRECTION('',(-1.,0.,0.));
#3630=DIRECTION('center_axis',(0.,-0.866025403784439,0.5));
#3631=DIRECTION('ref_axis',(0.,-0.5,-0.866025403784439));
#3632=DIRECTION('',(0.,0.5,0.866025403784439));
#3633=DIRECTION('',(0.,0.5,0.866025403784439));
#3634=DIRECTION('',(-1.,0.,0.));
#3635=DIRECTION('center_axis',(0.,-0.866025403784439,-0.5));
#3636=DIRECTION('ref_axis',(0.,0.5,-0.866025403784439));
#3637=DIRECTION('',(0.,-0.5,0.866025403784438));
#3638=DIRECTION('',(0.,-0.5,0.866025403784438));
#3639=DIRECTION('',(-1.,0.,0.));
#3640=DIRECTION('center_axis',(0.,-1.50231459873716E-16,-1.));
#3641=DIRECTION('ref_axis',(0.,1.,-1.50231459873716E-16));
#3642=DIRECTION('',(0.,-1.,1.50231459873716E-16));
#3643=DIRECTION('',(0.,-1.,1.50231459873716E-16));
#3644=DIRECTION('center_axis',(1.,0.,0.));
#3645=DIRECTION('ref_axis',(0.,0.,-1.));
#3646=DIRECTION('center_axis',(1.,0.,0.));
#3647=DIRECTION('ref_axis',(0.,0.,-1.));
#3648=DIRECTION('center_axis',(1.,0.,0.));
#3649=DIRECTION('ref_axis',(0.,0.,-1.));
#3650=DIRECTION('center_axis',(1.,0.,0.));
#3651=DIRECTION('ref_axis',(0.,0.,-1.));
#3652=DIRECTION('center_axis',(1.,0.,0.));
#3653=DIRECTION('ref_axis',(0.,0.,-1.));
#3654=DIRECTION('center_axis',(1.,0.,0.));
#3655=DIRECTION('ref_axis',(0.,0.,-1.));
#3656=DIRECTION('',(0.,0.,1.));
#3657=DIRECTION('',(1.,0.,0.));
#3658=DIRECTION('',(0.,0.,1.));
#3659=DIRECTION('',(1.,0.,0.));
#3660=DIRECTION('',(0.,0.,1.));
#3661=DIRECTION('',(1.,0.,0.));
#3662=DIRECTION('',(0.,0.,1.));
#3663=DIRECTION('',(1.,0.,0.));
#3664=DIRECTION('',(0.,0.,1.));
#3665=DIRECTION('',(1.,0.,0.));
#3666=DIRECTION('',(0.,0.,1.));
#3667=DIRECTION('',(1.,0.,0.));
#3668=DIRECTION('',(0.,0.,1.));
#3669=DIRECTION('',(1.,0.,0.));
#3670=DIRECTION('',(0.,0.,1.));
#3671=DIRECTION('',(1.,0.,0.));
#3672=DIRECTION('',(0.,0.,1.));
#3673=DIRECTION('',(0.,-1.,0.));
#3674=DIRECTION('',(0.,0.,1.));
#3675=DIRECTION('',(0.,-1.,0.));
#3676=DIRECTION('',(0.,0.,1.));
#3677=DIRECTION('',(0.,-1.,0.));
#3678=DIRECTION('',(0.,0.,1.));
#3679=DIRECTION('',(0.,-1.,0.));
#3680=CARTESIAN_POINT('',(0.,0.,0.));
#3681=CARTESIAN_POINT('',(0.,0.,0.));
#3682=CARTESIAN_POINT('Origin',(-6.66666666666667,0.,20.5));
#3683=CARTESIAN_POINT('',(-6.66666666666667,-1.20172123445289,20.5));
#3684=CARTESIAN_POINT('',(-6.66666666666667,0.,18.5));
#3685=CARTESIAN_POINT('',(-6.66666666666667,0.,18.5));
#3686=CARTESIAN_POINT('Origin',(-6.66666666666667,0.,20.5));
#3687=CARTESIAN_POINT('Origin',(-6.66666666666667,10.,20.5));
#3688=CARTESIAN_POINT('',(-6.66666666666667,10.,18.5));
#3689=CARTESIAN_POINT('',(-6.66666666666667,10.,18.5));
#3690=CARTESIAN_POINT('Origin',(-6.66666666666667,10.,20.5));
#3691=CARTESIAN_POINT('Origin',(6.66666666666666,0.,20.5));
#3692=CARTESIAN_POINT('',(6.66666666666666,-1.20172123445289,20.5));
#3693=CARTESIAN_POINT('',(6.66666666666666,0.,18.5));
#3694=CARTESIAN_POINT('',(6.66666666666666,0.,18.5));
#3695=CARTESIAN_POINT('Origin',(6.66666666666666,0.,20.5));
#3696=CARTESIAN_POINT('Origin',(6.66666666666666,10.,20.5));
#3697=CARTESIAN_POINT('',(6.66666666666666,10.,18.5));
#3698=CARTESIAN_POINT('',(6.66666666666666,10.,18.5));
#3699=CARTESIAN_POINT('Origin',(6.66666666666666,10.,20.5));
#3700=CARTESIAN_POINT('Origin',(6.66666666666666,0.,-20.5));
#3701=CARTESIAN_POINT('',(6.66666666666666,-1.20172123445289,-20.5));
#3702=CARTESIAN_POINT('',(6.66666666666666,0.,-22.5));
#3703=CARTESIAN_POINT('',(6.66666666666666,0.,-22.5));
#3704=CARTESIAN_POINT('Origin',(6.66666666666666,0.,-20.5));
#3705=CARTESIAN_POINT('Origin',(6.66666666666666,10.,-20.5));
#3706=CARTESIAN_POINT('',(6.66666666666666,10.,-22.5));
#3707=CARTESIAN_POINT('',(6.66666666666666,10.,-22.5));
#3708=CARTESIAN_POINT('Origin',(6.66666666666666,10.,-20.5));
#3709=CARTESIAN_POINT('Origin',(-6.66666666666667,0.,-20.5));
#3710=CARTESIAN_POINT('',(-6.66666666666667,-1.20172123445289,-20.5));
#3711=CARTESIAN_POINT('',(-6.66666666666667,0.,-22.5));
#3712=CARTESIAN_POINT('',(-6.66666666666667,0.,-22.5));
#3713=CARTESIAN_POINT('Origin',(-6.66666666666667,0.,-20.5));
#3714=CARTESIAN_POINT('Origin',(-6.66666666666667,10.,-20.5));
#3715=CARTESIAN_POINT('',(-6.66666666666667,10.,-22.5));
#3716=CARTESIAN_POINT('',(-6.66666666666667,10.,-22.5));
#3717=CARTESIAN_POINT('Origin',(-6.66666666666667,10.,-20.5));
#3718=CARTESIAN_POINT('Origin',(0.,-10.001,0.));
#3719=CARTESIAN_POINT('',(-4.,6.93889390390723E-15,0.));
#3720=CARTESIAN_POINT('',(4.,6.93889390390723E-15,0.));
#3721=CARTESIAN_POINT('Origin',(-5.44009282066327E-14,6.53255536936271E-14,
5.83866597897199E-14));
#3722=CARTESIAN_POINT('',(-4.8985871965897E-16,4.00000000000001,-4.));
#3723=CARTESIAN_POINT('Origin',(2.8461243742395E-14,-1.94289029309402E-14,
2.66453525910038E-14));
#3724=CARTESIAN_POINT('',(-4.89858719658941E-16,10.,-4.));
#3725=CARTESIAN_POINT('',(-4.89858719658941E-16,-10.001,-4.));
#3726=CARTESIAN_POINT('Origin',(0.,10.,0.));
#3727=CARTESIAN_POINT('Origin',(2.8461243742395E-14,-1.94289029309402E-14,
2.66453525910038E-14));
#3728=CARTESIAN_POINT('Origin',(-6.93889390390723E-15,6.93889390390723E-15,
25.));
#3729=CARTESIAN_POINT('',(3.99999999999999,0.,-5.));
#3730=CARTESIAN_POINT('',(-4.00000000000001,0.,-5.));
#3731=CARTESIAN_POINT('Origin',(-6.93889390390723E-15,6.93889390390723E-15,
-5.));
#3732=CARTESIAN_POINT('',(3.99999999999999,6.44903518424829E-15,-25.));
#3733=CARTESIAN_POINT('',(3.99999999999999,6.44903518424829E-15,25.));
#3734=CARTESIAN_POINT('Origin',(-6.93889390390723E-15,6.93889390390723E-15,
-25.));
#3735=CARTESIAN_POINT('',(3.99999999999999,0.,25.));
#3736=CARTESIAN_POINT('',(-4.00000000000001,0.,25.));
#3737=CARTESIAN_POINT('Origin',(-6.93889390390723E-15,6.93889390390723E-15,
25.));
#3738=CARTESIAN_POINT('',(3.99999999999999,6.44903518424829E-15,25.));
#3739=CARTESIAN_POINT('Origin',(-6.93889390390723E-15,6.93889390390723E-15,
25.));
#3740=CARTESIAN_POINT('',(3.99999999999999,0.,5.));
#3741=CARTESIAN_POINT('',(3.99999999999999,6.44903518424829E-15,25.));
#3742=CARTESIAN_POINT('',(-4.00000000000001,0.,5.));
#3743=CARTESIAN_POINT('Origin',(-6.93889390390723E-15,6.93889390390723E-15,
5.));
#3744=CARTESIAN_POINT('',(-4.00000000000001,0.,25.));
#3745=CARTESIAN_POINT('',(3.99999999999999,0.,25.));
#3746=CARTESIAN_POINT('Origin',(0.,0.,25.));
#3747=CARTESIAN_POINT('',(20.,-10.,25.));
#3748=CARTESIAN_POINT('',(20.,10.,25.));
#3749=CARTESIAN_POINT('',(20.,-10.,25.));
#3750=CARTESIAN_POINT('',(-20.,10.,25.));
#3751=CARTESIAN_POINT('',(-20.,10.,25.));
#3752=CARTESIAN_POINT('',(-20.,-10.,25.));
#3753=CARTESIAN_POINT('',(-20.,-10.,25.));
#3754=CARTESIAN_POINT('',(-20.,-10.,25.));
#3755=CARTESIAN_POINT('Origin',(0.,0.,-25.));
#3756=CARTESIAN_POINT('',(20.,-10.,-25.));
#3757=CARTESIAN_POINT('',(20.,10.,-25.));
#3758=CARTESIAN_POINT('',(20.,-10.,-25.));
#3759=CARTESIAN_POINT('',(-20.,-10.,-25.));
#3760=CARTESIAN_POINT('',(-20.,-10.,-25.));
#3761=CARTESIAN_POINT('',(-20.,10.,-25.));
#3762=CARTESIAN_POINT('',(-20.,-10.,-25.));
#3763=CARTESIAN_POINT('',(-20.,10.,-25.));
#3764=CARTESIAN_POINT('Origin',(20.,-10.,25.));
#3765=CARTESIAN_POINT('',(20.,10.,25.));
#3766=CARTESIAN_POINT('',(20.,-10.,25.));
#3767=CARTESIAN_POINT('Origin',(-20.,10.,25.));
#3768=CARTESIAN_POINT('',(-20.,10.,25.));
#3769=CARTESIAN_POINT('Origin',(-20.,-10.,25.));
#3770=CARTESIAN_POINT('',(-20.,-10.,25.));
#3771=CARTESIAN_POINT('Origin',(-20.,-10.,25.));
#3772=CARTESIAN_POINT('Origin',(-5.,0.,-5.));
#3773=CARTESIAN_POINT('',(-5.,0.,-5.));
#3774=CARTESIAN_POINT('Origin',(-5.,0.,5.));
#3775=CARTESIAN_POINT('',(-5.,0.,5.));
#3776=CARTESIAN_POINT('Origin',(0.,0.,0.));
#3777=CARTESIAN_POINT('',(0.,0.,0.));
#3778=CARTESIAN_POINT('Origin',(0.,15.,0.));
#3779=CARTESIAN_POINT('',(-6.12323399573677E-16,15.,-5.));
#3780=CARTESIAN_POINT('Origin',(0.,15.,0.));
#3781=CARTESIAN_POINT('',(-6.12323399573677E-16,33.,-5.));
#3782=CARTESIAN_POINT('',(-6.12323399573677E-16,15.,-5.));
#3783=CARTESIAN_POINT('Origin',(0.,33.,0.));
#3784=CARTESIAN_POINT('Origin',(0.,13.,0.));
#3785=CARTESIAN_POINT('',(-7.34788079488412E-16,33.,-6.));
#3786=CARTESIAN_POINT('Origin',(0.,33.,0.));
#3787=CARTESIAN_POINT('',(-7.34788079488412E-16,13.,-6.));
#3788=CARTESIAN_POINT('',(-7.34788079488412E-16,13.,-6.));
#3789=CARTESIAN_POINT('Origin',(0.,13.,0.));
#3790=CARTESIAN_POINT('Origin',(0.,5.,0.));
#3791=CARTESIAN_POINT('',(-3.06161699786838E-16,3.,2.5));
#3792=CARTESIAN_POINT('Origin',(0.,3.,0.));
#3793=CARTESIAN_POINT('',(-3.06161699786838E-16,5.,2.5));
#3794=CARTESIAN_POINT('',(-3.06161699786838E-16,5.,2.5));
#3795=CARTESIAN_POINT('Origin',(0.,5.,0.));
#3796=CARTESIAN_POINT('Origin',(0.,33.,0.));
#3797=CARTESIAN_POINT('',(-4.89858719658941E-16,5.,4.));
#3798=CARTESIAN_POINT('Origin',(0.,5.,0.));
#3799=CARTESIAN_POINT('',(-4.89858719658941E-16,13.,4.));
#3800=CARTESIAN_POINT('',(-4.89858719658941E-16,33.,4.));
#3801=CARTESIAN_POINT('Origin',(0.,13.,0.));
#3802=CARTESIAN_POINT('Origin',(0.,5.,0.));
#3803=CARTESIAN_POINT('Origin',(0.,3.,0.));
#3804=CARTESIAN_POINT('Origin',(0.,13.,0.));
#3805=CARTESIAN_POINT('Origin',(0.,33.,0.));
#3806=CARTESIAN_POINT('Origin',(0.,15.,0.));
#3807=CARTESIAN_POINT('',(0.,0.,0.));
#3808=CARTESIAN_POINT('Origin',(0.,3.,0.));
#3809=CARTESIAN_POINT('',(-3.06161699786838E-16,3.,-2.5));
#3810=CARTESIAN_POINT('Origin',(0.,3.,0.));
#3811=CARTESIAN_POINT('',(-3.06161699786838E-16,5.,-2.5));
#3812=CARTESIAN_POINT('',(-3.06161699786838E-16,3.,-2.5));
#3813=CARTESIAN_POINT('Origin',(0.,5.,0.));
#3814=CARTESIAN_POINT('Origin',(0.,3.,0.));
#3815=CARTESIAN_POINT('',(-4.89858719658941E-16,5.,-4.));
#3816=CARTESIAN_POINT('Origin',(0.,5.,0.));
#3817=CARTESIAN_POINT('',(-4.89858719658941E-16,0.,-4.));
#3818=CARTESIAN_POINT('',(-4.89858719658941E-16,3.,-4.));
#3819=CARTESIAN_POINT('Origin',(0.,0.,0.));
#3820=CARTESIAN_POINT('Origin',(0.,5.,0.));
#3821=CARTESIAN_POINT('Origin',(0.,3.,0.));
#3822=CARTESIAN_POINT('Origin',(0.,0.,0.));
#3823=CARTESIAN_POINT('',(0.,0.,0.));
#3824=CARTESIAN_POINT('Ctrl Pts',(-3.5,15.4968000776565,0.0564772772053689));
#3825=CARTESIAN_POINT('Ctrl Pts',(-3.51835057975363,15.6218000776565,-1.0807416596098));
#3826=CARTESIAN_POINT('Ctrl Pts',(-2.86475599094327,15.7468000776565,-2.01155730596849));
#3827=CARTESIAN_POINT('Ctrl Pts',(-2.2111614021329,15.8718000776565,-2.94237295232717));
#3828=CARTESIAN_POINT('Ctrl Pts',(-1.13527256282109,15.9968000776565,-3.31124536858055));
#3829=CARTESIAN_POINT('Ctrl Pts',(-0.0593837235092786,16.1218000776565,
-3.68011778483394));
#3830=CARTESIAN_POINT('Ctrl Pts',(1.02784639780354,16.2468000776565,-3.34615024548552));
#3831=CARTESIAN_POINT('Ctrl Pts',(2.11507651911636,16.3718000776565,-3.01218270613711));
#3832=CARTESIAN_POINT('Ctrl Pts',(2.79836296968137,16.4968000776565,-2.10293946007882));
#3833=CARTESIAN_POINT('Ctrl Pts',(3.48164942024637,16.6218000776565,-1.19369621402054));
#3834=CARTESIAN_POINT('Ctrl Pts',(3.5,16.7468000776565,-0.0564772772053694));
#3835=CARTESIAN_POINT('Ctrl Pts',(3.51835057975363,16.8718000776565,1.0807416596098));
#3836=CARTESIAN_POINT('Ctrl Pts',(2.86475599094327,16.9968000776565,2.01155730596849));
#3837=CARTESIAN_POINT('Ctrl Pts',(2.2111614021329,17.1218000776565,2.94237295232717));
#3838=CARTESIAN_POINT('Ctrl Pts',(1.13527256282109,17.2468000776565,3.31124536858055));
#3839=CARTESIAN_POINT('Ctrl Pts',(0.0593837235092791,17.3718000776565,3.68011778483394));
#3840=CARTESIAN_POINT('Ctrl Pts',(-1.02784639780354,17.4968000776565,3.34615024548552));
#3841=CARTESIAN_POINT('Ctrl Pts',(-2.11507651911636,17.6218000776565,3.01218270613711));
#3842=CARTESIAN_POINT('Ctrl Pts',(-2.79836296968137,17.7468000776565,2.10293946007882));
#3843=CARTESIAN_POINT('Ctrl Pts',(-3.48164942024637,17.8718000776565,1.19369621402054));
#3844=CARTESIAN_POINT('Ctrl Pts',(-3.5,17.9968000776565,0.0564772772053689));
#3845=CARTESIAN_POINT('Ctrl Pts',(-3.51835057975363,18.1218000776565,-1.0807416596098));
#3846=CARTESIAN_POINT('Ctrl Pts',(-2.86475599094327,18.2468000776565,-2.01155730596849));
#3847=CARTESIAN_POINT('Ctrl Pts',(-2.2111614021329,18.3718000776565,-2.94237295232717));
#3848=CARTESIAN_POINT('Ctrl Pts',(-1.13527256282109,18.4968000776565,-3.31124536858055));
#3849=CARTESIAN_POINT('Ctrl Pts',(-0.0593837235092786,18.6218000776565,
-3.68011778483394));
#3850=CARTESIAN_POINT('Ctrl Pts',(1.02784639780354,18.7468000776565,-3.34615024548552));
#3851=CARTESIAN_POINT('Ctrl Pts',(2.11507651911636,18.8718000776565,-3.01218270613711));
#3852=CARTESIAN_POINT('Ctrl Pts',(2.79836296968137,18.9968000776565,-2.10293946007882));
#3853=CARTESIAN_POINT('Ctrl Pts',(3.48164942024637,19.1218000776565,-1.19369621402054));
#3854=CARTESIAN_POINT('Ctrl Pts',(3.5,19.2468000776565,-0.0564772772053694));
#3855=CARTESIAN_POINT('Ctrl Pts',(3.51835057975363,19.3718000776565,1.0807416596098));
#3856=CARTESIAN_POINT('Ctrl Pts',(2.86475599094327,19.4968000776565,2.01155730596849));
#3857=CARTESIAN_POINT('Ctrl Pts',(2.2111614021329,19.6218000776565,2.94237295232717));
#3858=CARTESIAN_POINT('Ctrl Pts',(1.13527256282109,19.7468000776565,3.31124536858055));
#3859=CARTESIAN_POINT('Ctrl Pts',(0.0593837235092791,19.8718000776565,3.68011778483394));
#3860=CARTESIAN_POINT('Ctrl Pts',(-1.02784639780354,19.9968000776565,3.34615024548552));
#3861=CARTESIAN_POINT('Ctrl Pts',(-2.11507651911636,20.1218000776565,3.01218270613711));
#3862=CARTESIAN_POINT('Ctrl Pts',(-2.79836296968137,20.2468000776565,2.10293946007882));
#3863=CARTESIAN_POINT('Ctrl Pts',(-3.48164942024637,20.3718000776565,1.19369621402054));
#3864=CARTESIAN_POINT('Ctrl Pts',(-3.5,20.4968000776565,0.0564772772053689));
#3865=CARTESIAN_POINT('Ctrl Pts',(-3.51835057975363,20.6218000776565,-1.0807416596098));
#3866=CARTESIAN_POINT('Ctrl Pts',(-2.86475599094327,20.7468000776565,-2.01155730596849));
#3867=CARTESIAN_POINT('Ctrl Pts',(-2.2111614021329,20.8718000776565,-2.94237295232717));
#3868=CARTESIAN_POINT('Ctrl Pts',(-1.13527256282109,20.9968000776565,-3.31124536858055));
#3869=CARTESIAN_POINT('Ctrl Pts',(-0.0593837235092786,21.1218000776565,
-3.68011778483394));
#3870=CARTESIAN_POINT('Ctrl Pts',(1.02784639780354,21.2468000776565,-3.34615024548552));
#3871=CARTESIAN_POINT('Ctrl Pts',(2.11507651911636,21.3718000776565,-3.01218270613711));
#3872=CARTESIAN_POINT('Ctrl Pts',(2.79836296968137,21.4968000776565,-2.10293946007882));
#3873=CARTESIAN_POINT('Ctrl Pts',(3.48164942024637,21.6218000776565,-1.19369621402054));
#3874=CARTESIAN_POINT('Ctrl Pts',(3.5,21.7468000776565,-0.0564772772053694));
#3875=CARTESIAN_POINT('Ctrl Pts',(3.51835057975363,21.8718000776565,1.0807416596098));
#3876=CARTESIAN_POINT('Ctrl Pts',(2.86475599094327,21.9968000776565,2.01155730596849));
#3877=CARTESIAN_POINT('Ctrl Pts',(2.2111614021329,22.1218000776565,2.94237295232717));
#3878=CARTESIAN_POINT('Ctrl Pts',(1.13527256282109,22.2468000776565,3.31124536858055));
#3879=CARTESIAN_POINT('Ctrl Pts',(0.0593837235092791,22.3718000776565,3.68011778483394));
#3880=CARTESIAN_POINT('Ctrl Pts',(-1.02784639780354,22.4968000776565,3.34615024548552));
#3881=CARTESIAN_POINT('Ctrl Pts',(-2.11507651911636,22.6218000776565,3.01218270613711));
#3882=CARTESIAN_POINT('Ctrl Pts',(-2.79836296968137,22.7468000776565,2.10293946007882));
#3883=CARTESIAN_POINT('Ctrl Pts',(-3.48164942024637,22.8718000776565,1.19369621402054));
#3884=CARTESIAN_POINT('Ctrl Pts',(-3.5,22.9968000776565,0.0564772772053689));
#3885=CARTESIAN_POINT('Ctrl Pts',(-3.51835057975363,23.1218000776565,-1.0807416596098));
#3886=CARTESIAN_POINT('Ctrl Pts',(-2.86475599094327,23.2468000776565,-2.01155730596849));
#3887=CARTESIAN_POINT('Ctrl Pts',(-2.2111614021329,23.3718000776565,-2.94237295232717));
#3888=CARTESIAN_POINT('Ctrl Pts',(-1.13527256282109,23.4968000776565,-3.31124536858055));
#3889=CARTESIAN_POINT('Ctrl Pts',(-0.0593837235092786,23.6218000776565,
-3.68011778483394));
#3890=CARTESIAN_POINT('Ctrl Pts',(1.02784639780354,23.7468000776565,-3.34615024548552));
#3891=CARTESIAN_POINT('Ctrl Pts',(2.11507651911636,23.8718000776565,-3.01218270613711));
#3892=CARTESIAN_POINT('Ctrl Pts',(2.79836296968137,23.9968000776565,-2.10293946007882));
#3893=CARTESIAN_POINT('Ctrl Pts',(3.48164942024637,24.1218000776565,-1.19369621402054));
#3894=CARTESIAN_POINT('Ctrl Pts',(3.5,24.2468000776565,-0.0564772772053694));
#3895=CARTESIAN_POINT('Ctrl Pts',(3.51835057975363,24.3718000776565,1.0807416596098));
#3896=CARTESIAN_POINT('Ctrl Pts',(2.86475599094327,24.4968000776565,2.01155730596849));
#3897=CARTESIAN_POINT('Ctrl Pts',(2.2111614021329,24.6218000776565,2.94237295232717));
#3898=CARTESIAN_POINT('Ctrl Pts',(1.13527256282109,24.7468000776565,3.31124536858055));
#3899=CARTESIAN_POINT('Ctrl Pts',(0.0593837235092791,24.8718000776565,3.68011778483394));
#3900=CARTESIAN_POINT('Ctrl Pts',(-1.02784639780354,24.9968000776565,3.34615024548552));
#3901=CARTESIAN_POINT('Ctrl Pts',(-2.11507651911636,25.1218000776565,3.01218270613711));
#3902=CARTESIAN_POINT('Ctrl Pts',(-2.79836296968137,25.2468000776565,2.10293946007882));
#3903=CARTESIAN_POINT('Ctrl Pts',(-3.48164942024637,25.3718000776565,1.19369621402054));
#3904=CARTESIAN_POINT('Ctrl Pts',(-3.5,25.4968000776565,0.0564772772053689));
#3905=CARTESIAN_POINT('Ctrl Pts',(-3.51835057975363,25.6218000776565,-1.0807416596098));
#3906=CARTESIAN_POINT('Ctrl Pts',(-2.86475599094327,25.7468000776565,-2.01155730596849));
#3907=CARTESIAN_POINT('Ctrl Pts',(-2.2111614021329,25.8718000776565,-2.94237295232717));
#3908=CARTESIAN_POINT('Ctrl Pts',(-1.13527256282109,25.9968000776565,-3.31124536858055));
#3909=CARTESIAN_POINT('Ctrl Pts',(-0.0593837235092786,26.1218000776565,
-3.68011778483394));
#3910=CARTESIAN_POINT('Ctrl Pts',(1.02784639780354,26.2468000776565,-3.34615024548552));
#3911=CARTESIAN_POINT('Ctrl Pts',(2.11507651911636,26.3718000776565,-3.01218270613711));
#3912=CARTESIAN_POINT('Ctrl Pts',(2.79836296968137,26.4968000776565,-2.10293946007882));
#3913=CARTESIAN_POINT('Ctrl Pts',(3.48164942024637,26.6218000776565,-1.19369621402054));
#3914=CARTESIAN_POINT('Ctrl Pts',(3.5,26.7468000776565,-0.0564772772053694));
#3915=CARTESIAN_POINT('Ctrl Pts',(3.51835057975363,26.8718000776565,1.0807416596098));
#3916=CARTESIAN_POINT('Ctrl Pts',(2.86475599094327,26.9968000776565,2.01155730596849));
#3917=CARTESIAN_POINT('Ctrl Pts',(2.2111614021329,27.1218000776565,2.94237295232717));
#3918=CARTESIAN_POINT('Ctrl Pts',(1.13527256282109,27.2468000776565,3.31124536858055));
#3919=CARTESIAN_POINT('Ctrl Pts',(0.0593837235092791,27.3718000776565,3.68011778483394));
#3920=CARTESIAN_POINT('Ctrl Pts',(-1.02784639780354,27.4968000776565,3.34615024548552));
#3921=CARTESIAN_POINT('Ctrl Pts',(-2.11507651911636,27.6218000776565,3.01218270613711));
#3922=CARTESIAN_POINT('Ctrl Pts',(-2.79836296968137,27.7468000776565,2.10293946007882));
#3923=CARTESIAN_POINT('Ctrl Pts',(-3.48164942024637,27.8718000776565,1.19369621402054));
#3924=CARTESIAN_POINT('Ctrl Pts',(-3.5,27.9968000776565,0.0564772772053689));
#3925=CARTESIAN_POINT('Ctrl Pts',(-3.51835057975363,28.1218000776565,-1.0807416596098));
#3926=CARTESIAN_POINT('Ctrl Pts',(-2.86475599094327,28.2468000776565,-2.01155730596849));
#3927=CARTESIAN_POINT('Ctrl Pts',(-2.2111614021329,28.3718000776565,-2.94237295232717));
#3928=CARTESIAN_POINT('Ctrl Pts',(-1.13527256282109,28.4968000776565,-3.31124536858055));
#3929=CARTESIAN_POINT('Ctrl Pts',(-0.0593837235092786,28.6218000776565,
-3.68011778483394));
#3930=CARTESIAN_POINT('Ctrl Pts',(1.02784639780354,28.7468000776565,-3.34615024548552));
#3931=CARTESIAN_POINT('Ctrl Pts',(2.11507651911636,28.8718000776565,-3.01218270613711));
#3932=CARTESIAN_POINT('Ctrl Pts',(2.79836296968137,28.9968000776565,-2.10293946007882));
#3933=CARTESIAN_POINT('Ctrl Pts',(3.48164942024637,29.1218000776565,-1.19369621402054));
#3934=CARTESIAN_POINT('Ctrl Pts',(3.5,29.2468000776565,-0.0564772772053694));
#3935=CARTESIAN_POINT('Ctrl Pts',(3.51835057975363,29.3718000776565,1.0807416596098));
#3936=CARTESIAN_POINT('Ctrl Pts',(2.86475599094327,29.4968000776565,2.01155730596849));
#3937=CARTESIAN_POINT('Ctrl Pts',(2.2111614021329,29.6218000776565,2.94237295232717));
#3938=CARTESIAN_POINT('Ctrl Pts',(1.13527256282109,29.7468000776565,3.31124536858055));
#3939=CARTESIAN_POINT('Ctrl Pts',(0.0593837235092791,29.8718000776565,3.68011778483394));
#3940=CARTESIAN_POINT('Ctrl Pts',(-1.02784639780354,29.9968000776565,3.34615024548552));
#3941=CARTESIAN_POINT('Ctrl Pts',(-2.11507651911636,30.1218000776565,3.01218270613711));
#3942=CARTESIAN_POINT('Ctrl Pts',(-2.79836296968137,30.2468000776565,2.10293946007882));
#3943=CARTESIAN_POINT('Ctrl Pts',(-3.48164942024637,30.3718000776565,1.19369621402054));
#3944=CARTESIAN_POINT('Ctrl Pts',(-3.5,30.4968000776565,0.0564772772053689));
#3945=CARTESIAN_POINT('Ctrl Pts',(-3.51835057975363,30.6218000776565,-1.0807416596098));
#3946=CARTESIAN_POINT('Ctrl Pts',(-2.86475599094327,30.7468000776565,-2.01155730596849));
#3947=CARTESIAN_POINT('Ctrl Pts',(-2.2111614021329,30.8718000776565,-2.94237295232717));
#3948=CARTESIAN_POINT('Ctrl Pts',(-1.13527256282109,30.9968000776565,-3.31124536858055));
#3949=CARTESIAN_POINT('Ctrl Pts',(-0.0593837235092786,31.1218000776565,
-3.68011778483394));
#3950=CARTESIAN_POINT('Ctrl Pts',(1.02784639780354,31.2468000776565,-3.34615024548552));
#3951=CARTESIAN_POINT('Ctrl Pts',(2.11507651911636,31.3718000776565,-3.01218270613711));
#3952=CARTESIAN_POINT('Ctrl Pts',(2.79836296968137,31.4968000776565,-2.10293946007882));
#3953=CARTESIAN_POINT('Ctrl Pts',(3.48164942024637,31.6218000776565,-1.19369621402054));
#3954=CARTESIAN_POINT('Ctrl Pts',(3.5,31.7468000776565,-0.0564772772053694));
#3955=CARTESIAN_POINT('Ctrl Pts',(3.51835057975363,31.8718000776565,1.0807416596098));
#3956=CARTESIAN_POINT('Ctrl Pts',(2.86475599094327,31.9968000776565,2.01155730596849));
#3957=CARTESIAN_POINT('Ctrl Pts',(2.2111614021329,32.1218000776565,2.94237295232717));
#3958=CARTESIAN_POINT('Ctrl Pts',(1.13527256282109,32.2468000776565,3.31124536858055));
#3959=CARTESIAN_POINT('Ctrl Pts',(0.0593837235092791,32.3718000776565,3.68011778483394));
#3960=CARTESIAN_POINT('Ctrl Pts',(-1.02784639780354,32.4968000776565,3.34615024548552));
#3961=CARTESIAN_POINT('Ctrl Pts',(-2.11507651911636,32.6218000776565,3.01218270613711));
#3962=CARTESIAN_POINT('Ctrl Pts',(-2.79836296968137,32.7468000776565,2.10293946007882));
#3963=CARTESIAN_POINT('Ctrl Pts',(-3.48164942024637,32.8718000776565,1.19369621402054));
#3964=CARTESIAN_POINT('Ctrl Pts',(-3.5,32.9968000776565,0.0564772772053689));
#3965=CARTESIAN_POINT('Ctrl Pts',(-3.51835057975363,33.1218000776565,-1.0807416596098));
#3966=CARTESIAN_POINT('Ctrl Pts',(-2.86475599094327,33.2468000776565,-2.01155730596849));
#3967=CARTESIAN_POINT('Ctrl Pts',(-2.2111614021329,33.3718000776565,-2.94237295232717));
#3968=CARTESIAN_POINT('Ctrl Pts',(-1.13527256282109,33.4968000776565,-3.31124536858055));
#3969=CARTESIAN_POINT('Ctrl Pts',(-0.0593837235092786,33.6218000776565,
-3.68011778483394));
#3970=CARTESIAN_POINT('Ctrl Pts',(1.02784639780354,33.7468000776565,-3.34615024548552));
#3971=CARTESIAN_POINT('Ctrl Pts',(2.11507651911636,33.8718000776565,-3.01218270613711));
#3972=CARTESIAN_POINT('Ctrl Pts',(2.79836296968137,33.9968000776565,-2.10293946007882));
#3973=CARTESIAN_POINT('Ctrl Pts',(3.48164942024637,34.1218000776565,-1.19369621402054));
#3974=CARTESIAN_POINT('Ctrl Pts',(3.5,34.2468000776565,-0.0564772772053694));
#3975=CARTESIAN_POINT('Ctrl Pts',(3.51835057975363,34.3718000776565,1.0807416596098));
#3976=CARTESIAN_POINT('Ctrl Pts',(2.86475599094327,34.4968000776565,2.01155730596849));
#3977=CARTESIAN_POINT('Ctrl Pts',(2.2111614021329,34.6218000776565,2.94237295232717));
#3978=CARTESIAN_POINT('Ctrl Pts',(1.13527256282109,34.7468000776565,3.31124536858055));
#3979=CARTESIAN_POINT('Ctrl Pts',(0.0593837235092791,34.8718000776565,3.68011778483394));
#3980=CARTESIAN_POINT('Ctrl Pts',(-1.02784639780354,34.9968000776565,3.34615024548552));
#3981=CARTESIAN_POINT('Ctrl Pts',(-2.11507651911636,35.1218000776565,3.01218270613711));
#3982=CARTESIAN_POINT('Ctrl Pts',(-2.79836296968137,35.2468000776565,2.10293946007882));
#3983=CARTESIAN_POINT('Ctrl Pts',(-3.48164942024637,35.3718000776565,1.19369621402054));
#3984=CARTESIAN_POINT('Ctrl Pts',(-3.5,35.4968000776565,0.0564772772053689));
#3985=CARTESIAN_POINT('Ctrl Pts',(-3.51835057975363,35.6218000776565,-1.0807416596098));
#3986=CARTESIAN_POINT('Ctrl Pts',(-2.86475599094327,35.7468000776565,-2.01155730596849));
#3987=CARTESIAN_POINT('Ctrl Pts',(-2.2111614021329,35.8718000776565,-2.94237295232717));
#3988=CARTESIAN_POINT('Ctrl Pts',(-1.13527256282109,35.9968000776565,-3.31124536858055));
#3989=CARTESIAN_POINT('Ctrl Pts',(-0.0593837235092786,36.1218000776565,
-3.68011778483394));
#3990=CARTESIAN_POINT('Ctrl Pts',(1.02784639780354,36.2468000776565,-3.34615024548552));
#3991=CARTESIAN_POINT('Ctrl Pts',(2.11507651911636,36.3718000776565,-3.01218270613711));
#3992=CARTESIAN_POINT('Ctrl Pts',(2.79836296968137,36.4968000776565,-2.10293946007882));
#3993=CARTESIAN_POINT('Ctrl Pts',(3.48164942024637,36.6218000776565,-1.19369621402054));
#3994=CARTESIAN_POINT('Ctrl Pts',(3.5,36.7468000776565,-0.0564772772053694));
#3995=CARTESIAN_POINT('Ctrl Pts',(3.51835057975363,36.8718000776565,1.0807416596098));
#3996=CARTESIAN_POINT('Ctrl Pts',(2.86475599094327,36.9968000776565,2.01155730596849));
#3997=CARTESIAN_POINT('Ctrl Pts',(2.2111614021329,37.1218000776565,2.94237295232717));
#3998=CARTESIAN_POINT('Ctrl Pts',(1.13527256282109,37.2468000776565,3.31124536858055));
#3999=CARTESIAN_POINT('Ctrl Pts',(0.0593837235092791,37.3718000776565,3.68011778483394));
#4000=CARTESIAN_POINT('Ctrl Pts',(-1.02784639780354,37.4968000776565,3.34615024548552));
#4001=CARTESIAN_POINT('Ctrl Pts',(-2.11507651911636,37.6218000776565,3.01218270613711));
#4002=CARTESIAN_POINT('Ctrl Pts',(-2.79836296968137,37.7468000776565,2.10293946007882));
#4003=CARTESIAN_POINT('Ctrl Pts',(-3.48164942024637,37.8718000776565,1.19369621402054));
#4004=CARTESIAN_POINT('Ctrl Pts',(-3.5,37.9968000776565,0.0564772772053689));
#4005=CARTESIAN_POINT('Ctrl Pts',(-3.51835057975363,38.1218000776565,-1.0807416596098));
#4006=CARTESIAN_POINT('Ctrl Pts',(-2.86475599094327,38.2468000776565,-2.01155730596849));
#4007=CARTESIAN_POINT('Ctrl Pts',(-2.2111614021329,38.3718000776565,-2.94237295232717));
#4008=CARTESIAN_POINT('Ctrl Pts',(-1.13527256282109,38.4968000776565,-3.31124536858055));
#4009=CARTESIAN_POINT('Ctrl Pts',(-0.0593837235092786,38.6218000776565,
-3.68011778483394));
#4010=CARTESIAN_POINT('Ctrl Pts',(1.02784639780354,38.7468000776565,-3.34615024548552));
#4011=CARTESIAN_POINT('Ctrl Pts',(2.11507651911636,38.8718000776565,-3.01218270613711));
#4012=CARTESIAN_POINT('Ctrl Pts',(2.79836296968137,38.9968000776565,-2.10293946007882));
#4013=CARTESIAN_POINT('Ctrl Pts',(3.48164942024637,39.1218000776565,-1.19369621402054));
#4014=CARTESIAN_POINT('Ctrl Pts',(3.5,39.2468000776565,-0.0564772772053694));
#4015=CARTESIAN_POINT('Ctrl Pts',(3.51835057975363,39.3718000776565,1.0807416596098));
#4016=CARTESIAN_POINT('Ctrl Pts',(2.86475599094327,39.4968000776565,2.01155730596849));
#4017=CARTESIAN_POINT('Ctrl Pts',(2.2111614021329,39.6218000776565,2.94237295232717));
#4018=CARTESIAN_POINT('Ctrl Pts',(1.13527256282109,39.7468000776565,3.31124536858055));
#4019=CARTESIAN_POINT('Ctrl Pts',(0.0593837235092791,39.8718000776565,3.68011778483394));
#4020=CARTESIAN_POINT('Ctrl Pts',(-1.02784639780354,39.9968000776565,3.34615024548552));
#4021=CARTESIAN_POINT('Ctrl Pts',(-2.11507651911636,40.1218000776565,3.01218270613711));
#4022=CARTESIAN_POINT('Ctrl Pts',(-2.79836296968137,40.2468000776565,2.10293946007882));
#4023=CARTESIAN_POINT('Ctrl Pts',(-3.48164942024637,40.3718000776565,1.19369621402054));
#4024=CARTESIAN_POINT('Ctrl Pts',(-3.5,40.4968000776565,0.0564772772053689));
#4025=CARTESIAN_POINT('Ctrl Pts',(-2.5,15.4968000776565,0.0564772772053586));
#4026=CARTESIAN_POINT('Ctrl Pts',(-2.51835057975363,15.6218000776565,-0.755821963376908));
#4027=CARTESIAN_POINT('Ctrl Pts',(-2.05573899656831,15.7468000776565,-1.42377205367602));
#4028=CARTESIAN_POINT('Ctrl Pts',(-1.593127413383,15.8718000776565,-2.09172214397514));
#4029=CARTESIAN_POINT('Ctrl Pts',(-0.826255568446133,15.9968000776565,-2.3601888522854));
#4030=CARTESIAN_POINT('Ctrl Pts',(-0.0593837235092677,16.1218000776565,
-2.62865556059567));
#4031=CARTESIAN_POINT('Ctrl Pts',(0.718829403428605,16.2468000776565,-2.39509372919037));
#4032=CARTESIAN_POINT('Ctrl Pts',(1.49704253036648,16.3718000776565,-2.16153189778506));
#4033=CARTESIAN_POINT('Ctrl Pts',(1.98934597530643,16.4968000776565,-1.51515420778634));
#4034=CARTESIAN_POINT('Ctrl Pts',(2.48164942024637,16.6218000776565,-0.868776517787625));
#4035=CARTESIAN_POINT('Ctrl Pts',(2.5,16.7468000776565,-0.0564772772053589));
#4036=CARTESIAN_POINT('Ctrl Pts',(2.51835057975363,16.8718000776565,0.755821963376907));
#4037=CARTESIAN_POINT('Ctrl Pts',(2.05573899656831,16.9968000776565,1.42377205367602));
#4038=CARTESIAN_POINT('Ctrl Pts',(1.593127413383,17.1218000776565,2.09172214397514));
#4039=CARTESIAN_POINT('Ctrl Pts',(0.826255568446133,17.2468000776565,2.3601888522854));
#4040=CARTESIAN_POINT('Ctrl Pts',(0.059383723509268,17.3718000776565,2.62865556059567));
#4041=CARTESIAN_POINT('Ctrl Pts',(-0.718829403428604,17.4968000776565,2.39509372919037));
#4042=CARTESIAN_POINT('Ctrl Pts',(-1.49704253036648,17.6218000776565,2.16153189778506));
#4043=CARTESIAN_POINT('Ctrl Pts',(-1.98934597530643,17.7468000776565,1.51515420778634));
#4044=CARTESIAN_POINT('Ctrl Pts',(-2.48164942024637,17.8718000776565,0.868776517787626));
#4045=CARTESIAN_POINT('Ctrl Pts',(-2.5,17.9968000776565,0.0564772772053586));
#4046=CARTESIAN_POINT('Ctrl Pts',(-2.51835057975363,18.1218000776565,-0.755821963376908));
#4047=CARTESIAN_POINT('Ctrl Pts',(-2.05573899656831,18.2468000776565,-1.42377205367602));
#4048=CARTESIAN_POINT('Ctrl Pts',(-1.593127413383,18.3718000776565,-2.09172214397514));
#4049=CARTESIAN_POINT('Ctrl Pts',(-0.826255568446133,18.4968000776565,-2.3601888522854));
#4050=CARTESIAN_POINT('Ctrl Pts',(-0.0593837235092677,18.6218000776565,
-2.62865556059567));
#4051=CARTESIAN_POINT('Ctrl Pts',(0.718829403428605,18.7468000776565,-2.39509372919037));
#4052=CARTESIAN_POINT('Ctrl Pts',(1.49704253036648,18.8718000776565,-2.16153189778506));
#4053=CARTESIAN_POINT('Ctrl Pts',(1.98934597530643,18.9968000776565,-1.51515420778634));
#4054=CARTESIAN_POINT('Ctrl Pts',(2.48164942024637,19.1218000776565,-0.868776517787625));
#4055=CARTESIAN_POINT('Ctrl Pts',(2.5,19.2468000776565,-0.0564772772053589));
#4056=CARTESIAN_POINT('Ctrl Pts',(2.51835057975363,19.3718000776565,0.755821963376907));
#4057=CARTESIAN_POINT('Ctrl Pts',(2.05573899656831,19.4968000776565,1.42377205367602));
#4058=CARTESIAN_POINT('Ctrl Pts',(1.593127413383,19.6218000776565,2.09172214397514));
#4059=CARTESIAN_POINT('Ctrl Pts',(0.826255568446133,19.7468000776565,2.3601888522854));
#4060=CARTESIAN_POINT('Ctrl Pts',(0.059383723509268,19.8718000776565,2.62865556059567));
#4061=CARTESIAN_POINT('Ctrl Pts',(-0.718829403428604,19.9968000776565,2.39509372919037));
#4062=CARTESIAN_POINT('Ctrl Pts',(-1.49704253036648,20.1218000776565,2.16153189778506));
#4063=CARTESIAN_POINT('Ctrl Pts',(-1.98934597530643,20.2468000776565,1.51515420778634));
#4064=CARTESIAN_POINT('Ctrl Pts',(-2.48164942024637,20.3718000776565,0.868776517787626));
#4065=CARTESIAN_POINT('Ctrl Pts',(-2.5,20.4968000776565,0.0564772772053586));
#4066=CARTESIAN_POINT('Ctrl Pts',(-2.51835057975363,20.6218000776565,-0.755821963376908));
#4067=CARTESIAN_POINT('Ctrl Pts',(-2.05573899656831,20.7468000776565,-1.42377205367602));
#4068=CARTESIAN_POINT('Ctrl Pts',(-1.593127413383,20.8718000776565,-2.09172214397514));
#4069=CARTESIAN_POINT('Ctrl Pts',(-0.826255568446133,20.9968000776565,-2.3601888522854));
#4070=CARTESIAN_POINT('Ctrl Pts',(-0.0593837235092677,21.1218000776565,
-2.62865556059567));
#4071=CARTESIAN_POINT('Ctrl Pts',(0.718829403428605,21.2468000776565,-2.39509372919037));
#4072=CARTESIAN_POINT('Ctrl Pts',(1.49704253036648,21.3718000776565,-2.16153189778506));
#4073=CARTESIAN_POINT('Ctrl Pts',(1.98934597530643,21.4968000776565,-1.51515420778634));
#4074=CARTESIAN_POINT('Ctrl Pts',(2.48164942024637,21.6218000776565,-0.868776517787625));
#4075=CARTESIAN_POINT('Ctrl Pts',(2.5,21.7468000776565,-0.0564772772053589));
#4076=CARTESIAN_POINT('Ctrl Pts',(2.51835057975363,21.8718000776565,0.755821963376907));
#4077=CARTESIAN_POINT('Ctrl Pts',(2.05573899656831,21.9968000776565,1.42377205367602));
#4078=CARTESIAN_POINT('Ctrl Pts',(1.593127413383,22.1218000776565,2.09172214397514));
#4079=CARTESIAN_POINT('Ctrl Pts',(0.826255568446133,22.2468000776565,2.3601888522854));
#4080=CARTESIAN_POINT('Ctrl Pts',(0.059383723509268,22.3718000776565,2.62865556059567));
#4081=CARTESIAN_POINT('Ctrl Pts',(-0.718829403428604,22.4968000776565,2.39509372919037));
#4082=CARTESIAN_POINT('Ctrl Pts',(-1.49704253036648,22.6218000776565,2.16153189778506));
#4083=CARTESIAN_POINT('Ctrl Pts',(-1.98934597530643,22.7468000776565,1.51515420778634));
#4084=CARTESIAN_POINT('Ctrl Pts',(-2.48164942024637,22.8718000776565,0.868776517787626));
#4085=CARTESIAN_POINT('Ctrl Pts',(-2.5,22.9968000776565,0.0564772772053586));
#4086=CARTESIAN_POINT('Ctrl Pts',(-2.51835057975363,23.1218000776565,-0.755821963376908));
#4087=CARTESIAN_POINT('Ctrl Pts',(-2.05573899656831,23.2468000776565,-1.42377205367602));
#4088=CARTESIAN_POINT('Ctrl Pts',(-1.593127413383,23.3718000776565,-2.09172214397514));
#4089=CARTESIAN_POINT('Ctrl Pts',(-0.826255568446133,23.4968000776565,-2.3601888522854));
#4090=CARTESIAN_POINT('Ctrl Pts',(-0.0593837235092677,23.6218000776565,
-2.62865556059567));
#4091=CARTESIAN_POINT('Ctrl Pts',(0.718829403428605,23.7468000776565,-2.39509372919037));
#4092=CARTESIAN_POINT('Ctrl Pts',(1.49704253036648,23.8718000776565,-2.16153189778506));
#4093=CARTESIAN_POINT('Ctrl Pts',(1.98934597530643,23.9968000776565,-1.51515420778634));
#4094=CARTESIAN_POINT('Ctrl Pts',(2.48164942024637,24.1218000776565,-0.868776517787625));
#4095=CARTESIAN_POINT('Ctrl Pts',(2.5,24.2468000776565,-0.0564772772053589));
#4096=CARTESIAN_POINT('Ctrl Pts',(2.51835057975363,24.3718000776565,0.755821963376907));
#4097=CARTESIAN_POINT('Ctrl Pts',(2.05573899656831,24.4968000776565,1.42377205367602));
#4098=CARTESIAN_POINT('Ctrl Pts',(1.593127413383,24.6218000776565,2.09172214397514));
#4099=CARTESIAN_POINT('Ctrl Pts',(0.826255568446133,24.7468000776565,2.3601888522854));
#4100=CARTESIAN_POINT('Ctrl Pts',(0.059383723509268,24.8718000776565,2.62865556059567));
#4101=CARTESIAN_POINT('Ctrl Pts',(-0.718829403428604,24.9968000776565,2.39509372919037));
#4102=CARTESIAN_POINT('Ctrl Pts',(-1.49704253036648,25.1218000776565,2.16153189778506));
#4103=CARTESIAN_POINT('Ctrl Pts',(-1.98934597530643,25.2468000776565,1.51515420778634));
#4104=CARTESIAN_POINT('Ctrl Pts',(-2.48164942024637,25.3718000776565,0.868776517787626));
#4105=CARTESIAN_POINT('Ctrl Pts',(-2.5,25.4968000776565,0.0564772772053586));
#4106=CARTESIAN_POINT('Ctrl Pts',(-2.51835057975363,25.6218000776565,-0.755821963376908));
#4107=CARTESIAN_POINT('Ctrl Pts',(-2.05573899656831,25.7468000776565,-1.42377205367602));
#4108=CARTESIAN_POINT('Ctrl Pts',(-1.593127413383,25.8718000776565,-2.09172214397514));
#4109=CARTESIAN_POINT('Ctrl Pts',(-0.826255568446133,25.9968000776565,-2.3601888522854));
#4110=CARTESIAN_POINT('Ctrl Pts',(-0.0593837235092677,26.1218000776565,
-2.62865556059567));
#4111=CARTESIAN_POINT('Ctrl Pts',(0.718829403428605,26.2468000776565,-2.39509372919037));
#4112=CARTESIAN_POINT('Ctrl Pts',(1.49704253036648,26.3718000776565,-2.16153189778506));
#4113=CARTESIAN_POINT('Ctrl Pts',(1.98934597530643,26.4968000776565,-1.51515420778634));
#4114=CARTESIAN_POINT('Ctrl Pts',(2.48164942024637,26.6218000776565,-0.868776517787625));
#4115=CARTESIAN_POINT('Ctrl Pts',(2.5,26.7468000776565,-0.0564772772053589));
#4116=CARTESIAN_POINT('Ctrl Pts',(2.51835057975363,26.8718000776565,0.755821963376907));
#4117=CARTESIAN_POINT('Ctrl Pts',(2.05573899656831,26.9968000776565,1.42377205367602));
#4118=CARTESIAN_POINT('Ctrl Pts',(1.593127413383,27.1218000776565,2.09172214397514));
#4119=CARTESIAN_POINT('Ctrl Pts',(0.826255568446133,27.2468000776565,2.3601888522854));
#4120=CARTESIAN_POINT('Ctrl Pts',(0.059383723509268,27.3718000776565,2.62865556059567));
#4121=CARTESIAN_POINT('Ctrl Pts',(-0.718829403428604,27.4968000776565,2.39509372919037));
#4122=CARTESIAN_POINT('Ctrl Pts',(-1.49704253036648,27.6218000776565,2.16153189778506));
#4123=CARTESIAN_POINT('Ctrl Pts',(-1.98934597530643,27.7468000776565,1.51515420778634));
#4124=CARTESIAN_POINT('Ctrl Pts',(-2.48164942024637,27.8718000776565,0.868776517787626));
#4125=CARTESIAN_POINT('Ctrl Pts',(-2.5,27.9968000776565,0.0564772772053586));
#4126=CARTESIAN_POINT('Ctrl Pts',(-2.51835057975363,28.1218000776565,-0.755821963376908));
#4127=CARTESIAN_POINT('Ctrl Pts',(-2.05573899656831,28.2468000776565,-1.42377205367602));
#4128=CARTESIAN_POINT('Ctrl Pts',(-1.593127413383,28.3718000776565,-2.09172214397514));
#4129=CARTESIAN_POINT('Ctrl Pts',(-0.826255568446133,28.4968000776565,-2.3601888522854));
#4130=CARTESIAN_POINT('Ctrl Pts',(-0.0593837235092677,28.6218000776565,
-2.62865556059567));
#4131=CARTESIAN_POINT('Ctrl Pts',(0.718829403428605,28.7468000776565,-2.39509372919037));
#4132=CARTESIAN_POINT('Ctrl Pts',(1.49704253036648,28.8718000776565,-2.16153189778506));
#4133=CARTESIAN_POINT('Ctrl Pts',(1.98934597530643,28.9968000776565,-1.51515420778634));
#4134=CARTESIAN_POINT('Ctrl Pts',(2.48164942024637,29.1218000776565,-0.868776517787625));
#4135=CARTESIAN_POINT('Ctrl Pts',(2.5,29.2468000776565,-0.0564772772053589));
#4136=CARTESIAN_POINT('Ctrl Pts',(2.51835057975363,29.3718000776565,0.755821963376907));
#4137=CARTESIAN_POINT('Ctrl Pts',(2.05573899656831,29.4968000776565,1.42377205367602));
#4138=CARTESIAN_POINT('Ctrl Pts',(1.593127413383,29.6218000776565,2.09172214397514));
#4139=CARTESIAN_POINT('Ctrl Pts',(0.826255568446133,29.7468000776565,2.3601888522854));
#4140=CARTESIAN_POINT('Ctrl Pts',(0.059383723509268,29.8718000776565,2.62865556059567));
#4141=CARTESIAN_POINT('Ctrl Pts',(-0.718829403428604,29.9968000776565,2.39509372919037));
#4142=CARTESIAN_POINT('Ctrl Pts',(-1.49704253036648,30.1218000776565,2.16153189778506));
#4143=CARTESIAN_POINT('Ctrl Pts',(-1.98934597530643,30.2468000776565,1.51515420778634));
#4144=CARTESIAN_POINT('Ctrl Pts',(-2.48164942024637,30.3718000776565,0.868776517787626));
#4145=CARTESIAN_POINT('Ctrl Pts',(-2.5,30.4968000776565,0.0564772772053586));
#4146=CARTESIAN_POINT('Ctrl Pts',(-2.51835057975363,30.6218000776565,-0.755821963376908));
#4147=CARTESIAN_POINT('Ctrl Pts',(-2.05573899656831,30.7468000776565,-1.42377205367602));
#4148=CARTESIAN_POINT('Ctrl Pts',(-1.593127413383,30.8718000776565,-2.09172214397514));
#4149=CARTESIAN_POINT('Ctrl Pts',(-0.826255568446133,30.9968000776565,-2.3601888522854));
#4150=CARTESIAN_POINT('Ctrl Pts',(-0.0593837235092677,31.1218000776565,
-2.62865556059567));
#4151=CARTESIAN_POINT('Ctrl Pts',(0.718829403428605,31.2468000776565,-2.39509372919037));
#4152=CARTESIAN_POINT('Ctrl Pts',(1.49704253036648,31.3718000776565,-2.16153189778506));
#4153=CARTESIAN_POINT('Ctrl Pts',(1.98934597530643,31.4968000776565,-1.51515420778634));
#4154=CARTESIAN_POINT('Ctrl Pts',(2.48164942024637,31.6218000776565,-0.868776517787625));
#4155=CARTESIAN_POINT('Ctrl Pts',(2.5,31.7468000776565,-0.0564772772053589));
#4156=CARTESIAN_POINT('Ctrl Pts',(2.51835057975363,31.8718000776565,0.755821963376907));
#4157=CARTESIAN_POINT('Ctrl Pts',(2.05573899656831,31.9968000776565,1.42377205367602));
#4158=CARTESIAN_POINT('Ctrl Pts',(1.593127413383,32.1218000776565,2.09172214397514));
#4159=CARTESIAN_POINT('Ctrl Pts',(0.826255568446133,32.2468000776565,2.3601888522854));
#4160=CARTESIAN_POINT('Ctrl Pts',(0.059383723509268,32.3718000776565,2.62865556059567));
#4161=CARTESIAN_POINT('Ctrl Pts',(-0.718829403428604,32.4968000776565,2.39509372919037));
#4162=CARTESIAN_POINT('Ctrl Pts',(-1.49704253036648,32.6218000776565,2.16153189778506));
#4163=CARTESIAN_POINT('Ctrl Pts',(-1.98934597530643,32.7468000776565,1.51515420778634));
#4164=CARTESIAN_POINT('Ctrl Pts',(-2.48164942024637,32.8718000776565,0.868776517787626));
#4165=CARTESIAN_POINT('Ctrl Pts',(-2.5,32.9968000776565,0.0564772772053586));
#4166=CARTESIAN_POINT('Ctrl Pts',(-2.51835057975363,33.1218000776565,-0.755821963376908));
#4167=CARTESIAN_POINT('Ctrl Pts',(-2.05573899656831,33.2468000776565,-1.42377205367602));
#4168=CARTESIAN_POINT('Ctrl Pts',(-1.593127413383,33.3718000776565,-2.09172214397514));
#4169=CARTESIAN_POINT('Ctrl Pts',(-0.826255568446133,33.4968000776565,-2.3601888522854));
#4170=CARTESIAN_POINT('Ctrl Pts',(-0.0593837235092677,33.6218000776565,
-2.62865556059567));
#4171=CARTESIAN_POINT('Ctrl Pts',(0.718829403428605,33.7468000776565,-2.39509372919037));
#4172=CARTESIAN_POINT('Ctrl Pts',(1.49704253036648,33.8718000776565,-2.16153189778506));
#4173=CARTESIAN_POINT('Ctrl Pts',(1.98934597530643,33.9968000776565,-1.51515420778634));
#4174=CARTESIAN_POINT('Ctrl Pts',(2.48164942024637,34.1218000776565,-0.868776517787625));
#4175=CARTESIAN_POINT('Ctrl Pts',(2.5,34.2468000776565,-0.0564772772053589));
#4176=CARTESIAN_POINT('Ctrl Pts',(2.51835057975363,34.3718000776565,0.755821963376907));
#4177=CARTESIAN_POINT('Ctrl Pts',(2.05573899656831,34.4968000776565,1.42377205367602));
#4178=CARTESIAN_POINT('Ctrl Pts',(1.593127413383,34.6218000776565,2.09172214397514));
#4179=CARTESIAN_POINT('Ctrl Pts',(0.826255568446133,34.7468000776565,2.3601888522854));
#4180=CARTESIAN_POINT('Ctrl Pts',(0.059383723509268,34.8718000776565,2.62865556059567));
#4181=CARTESIAN_POINT('Ctrl Pts',(-0.718829403428604,34.9968000776565,2.39509372919037));
#4182=CARTESIAN_POINT('Ctrl Pts',(-1.49704253036648,35.1218000776565,2.16153189778506));
#4183=CARTESIAN_POINT('Ctrl Pts',(-1.98934597530643,35.2468000776565,1.51515420778634));
#4184=CARTESIAN_POINT('Ctrl Pts',(-2.48164942024637,35.3718000776565,0.868776517787626));
#4185=CARTESIAN_POINT('Ctrl Pts',(-2.5,35.4968000776565,0.0564772772053586));
#4186=CARTESIAN_POINT('Ctrl Pts',(-2.51835057975363,35.6218000776565,-0.755821963376908));
#4187=CARTESIAN_POINT('Ctrl Pts',(-2.05573899656831,35.7468000776565,-1.42377205367602));
#4188=CARTESIAN_POINT('Ctrl Pts',(-1.593127413383,35.8718000776565,-2.09172214397514));
#4189=CARTESIAN_POINT('Ctrl Pts',(-0.826255568446133,35.9968000776565,-2.3601888522854));
#4190=CARTESIAN_POINT('Ctrl Pts',(-0.0593837235092677,36.1218000776565,
-2.62865556059567));
#4191=CARTESIAN_POINT('Ctrl Pts',(0.718829403428605,36.2468000776565,-2.39509372919037));
#4192=CARTESIAN_POINT('Ctrl Pts',(1.49704253036648,36.3718000776565,-2.16153189778506));
#4193=CARTESIAN_POINT('Ctrl Pts',(1.98934597530643,36.4968000776565,-1.51515420778634));
#4194=CARTESIAN_POINT('Ctrl Pts',(2.48164942024637,36.6218000776565,-0.868776517787625));
#4195=CARTESIAN_POINT('Ctrl Pts',(2.5,36.7468000776565,-0.0564772772053589));
#4196=CARTESIAN_POINT('Ctrl Pts',(2.51835057975363,36.8718000776565,0.755821963376907));
#4197=CARTESIAN_POINT('Ctrl Pts',(2.05573899656831,36.9968000776565,1.42377205367602));
#4198=CARTESIAN_POINT('Ctrl Pts',(1.593127413383,37.1218000776565,2.09172214397514));
#4199=CARTESIAN_POINT('Ctrl Pts',(0.826255568446133,37.2468000776565,2.3601888522854));
#4200=CARTESIAN_POINT('Ctrl Pts',(0.059383723509268,37.3718000776565,2.62865556059567));
#4201=CARTESIAN_POINT('Ctrl Pts',(-0.718829403428604,37.4968000776565,2.39509372919037));
#4202=CARTESIAN_POINT('Ctrl Pts',(-1.49704253036648,37.6218000776565,2.16153189778506));
#4203=CARTESIAN_POINT('Ctrl Pts',(-1.98934597530643,37.7468000776565,1.51515420778634));
#4204=CARTESIAN_POINT('Ctrl Pts',(-2.48164942024637,37.8718000776565,0.868776517787626));
#4205=CARTESIAN_POINT('Ctrl Pts',(-2.5,37.9968000776565,0.0564772772053586));
#4206=CARTESIAN_POINT('Ctrl Pts',(-2.51835057975363,38.1218000776565,-0.755821963376908));
#4207=CARTESIAN_POINT('Ctrl Pts',(-2.05573899656831,38.2468000776565,-1.42377205367602));
#4208=CARTESIAN_POINT('Ctrl Pts',(-1.593127413383,38.3718000776565,-2.09172214397514));
#4209=CARTESIAN_POINT('Ctrl Pts',(-0.826255568446133,38.4968000776565,-2.3601888522854));
#4210=CARTESIAN_POINT('Ctrl Pts',(-0.0593837235092677,38.6218000776565,
-2.62865556059567));
#4211=CARTESIAN_POINT('Ctrl Pts',(0.718829403428605,38.7468000776565,-2.39509372919037));
#4212=CARTESIAN_POINT('Ctrl Pts',(1.49704253036648,38.8718000776565,-2.16153189778506));
#4213=CARTESIAN_POINT('Ctrl Pts',(1.98934597530643,38.9968000776565,-1.51515420778634));
#4214=CARTESIAN_POINT('Ctrl Pts',(2.48164942024637,39.1218000776565,-0.868776517787625));
#4215=CARTESIAN_POINT('Ctrl Pts',(2.5,39.2468000776565,-0.0564772772053589));
#4216=CARTESIAN_POINT('Ctrl Pts',(2.51835057975363,39.3718000776565,0.755821963376907));
#4217=CARTESIAN_POINT('Ctrl Pts',(2.05573899656831,39.4968000776565,1.42377205367602));
#4218=CARTESIAN_POINT('Ctrl Pts',(1.593127413383,39.6218000776565,2.09172214397514));
#4219=CARTESIAN_POINT('Ctrl Pts',(0.826255568446133,39.7468000776565,2.3601888522854));
#4220=CARTESIAN_POINT('Ctrl Pts',(0.059383723509268,39.8718000776565,2.62865556059567));
#4221=CARTESIAN_POINT('Ctrl Pts',(-0.718829403428604,39.9968000776565,2.39509372919037));
#4222=CARTESIAN_POINT('Ctrl Pts',(-1.49704253036648,40.1218000776565,2.16153189778506));
#4223=CARTESIAN_POINT('Ctrl Pts',(-1.98934597530643,40.2468000776565,1.51515420778634));
#4224=CARTESIAN_POINT('Ctrl Pts',(-2.48164942024637,40.3718000776565,0.868776517787626));
#4225=CARTESIAN_POINT('Ctrl Pts',(-2.5,40.4968000776565,0.0564772772053586));
#4226=CARTESIAN_POINT('Ctrl Pts',(-2.5,14.5031999223435,-0.056477277205306));
#4227=CARTESIAN_POINT('Ctrl Pts',(-2.48164942024639,14.6281999223435,-0.868776517787572));
#4228=CARTESIAN_POINT('Ctrl Pts',(-1.98934597530646,14.7531999223435,-1.5151542077863));
#4229=CARTESIAN_POINT('Ctrl Pts',(-1.49704253036652,14.8781999223435,-2.16153189778503));
#4230=CARTESIAN_POINT('Ctrl Pts',(-0.718829403428655,15.0031999223435,-2.39509372919035));
#4231=CARTESIAN_POINT('Ctrl Pts',(0.0593837235092121,15.1281999223435,-2.62865556059567));
#4232=CARTESIAN_POINT('Ctrl Pts',(0.826255568446083,15.2531999223435,-2.36018885228542));
#4233=CARTESIAN_POINT('Ctrl Pts',(1.59312741338295,15.3781999223435,-2.09172214397517));
#4234=CARTESIAN_POINT('Ctrl Pts',(2.05573899656828,15.5031999223436,-1.42377205367607));
#4235=CARTESIAN_POINT('Ctrl Pts',(2.51835057975361,15.6281999223435,-0.755821963376961));
#4236=CARTESIAN_POINT('Ctrl Pts',(2.5,15.7531999223435,0.0564772772053057));
#4237=CARTESIAN_POINT('Ctrl Pts',(2.48164942024639,15.8781999223435,0.868776517787572));
#4238=CARTESIAN_POINT('Ctrl Pts',(1.98934597530646,16.0031999223435,1.5151542077863));
#4239=CARTESIAN_POINT('Ctrl Pts',(1.49704253036652,16.1281999223435,2.16153189778503));
#4240=CARTESIAN_POINT('Ctrl Pts',(0.718829403428655,16.2531999223435,2.39509372919035));
#4241=CARTESIAN_POINT('Ctrl Pts',(-0.0593837235092117,16.3781999223435,
2.62865556059567));
#4242=CARTESIAN_POINT('Ctrl Pts',(-0.826255568446083,16.5031999223435,2.36018885228542));
#4243=CARTESIAN_POINT('Ctrl Pts',(-1.59312741338295,16.6281999223435,2.09172214397517));
#4244=CARTESIAN_POINT('Ctrl Pts',(-2.05573899656828,16.7531999223435,1.42377205367607));
#4245=CARTESIAN_POINT('Ctrl Pts',(-2.51835057975361,16.8781999223435,0.755821963376961));
#4246=CARTESIAN_POINT('Ctrl Pts',(-2.5,17.0031999223435,-0.056477277205306));
#4247=CARTESIAN_POINT('Ctrl Pts',(-2.48164942024639,17.1281999223435,-0.868776517787572));
#4248=CARTESIAN_POINT('Ctrl Pts',(-1.98934597530646,17.2531999223435,-1.5151542077863));
#4249=CARTESIAN_POINT('Ctrl Pts',(-1.49704253036652,17.3781999223435,-2.16153189778503));
#4250=CARTESIAN_POINT('Ctrl Pts',(-0.718829403428655,17.5031999223435,-2.39509372919035));
#4251=CARTESIAN_POINT('Ctrl Pts',(0.0593837235092121,17.6281999223435,-2.62865556059567));
#4252=CARTESIAN_POINT('Ctrl Pts',(0.826255568446083,17.7531999223435,-2.36018885228542));
#4253=CARTESIAN_POINT('Ctrl Pts',(1.59312741338295,17.8781999223435,-2.09172214397517));
#4254=CARTESIAN_POINT('Ctrl Pts',(2.05573899656828,18.0031999223435,-1.42377205367607));
#4255=CARTESIAN_POINT('Ctrl Pts',(2.51835057975361,18.1281999223435,-0.755821963376961));
#4256=CARTESIAN_POINT('Ctrl Pts',(2.5,18.2531999223435,0.0564772772053057));
#4257=CARTESIAN_POINT('Ctrl Pts',(2.48164942024639,18.3781999223435,0.868776517787572));
#4258=CARTESIAN_POINT('Ctrl Pts',(1.98934597530646,18.5031999223435,1.5151542077863));
#4259=CARTESIAN_POINT('Ctrl Pts',(1.49704253036652,18.6281999223435,2.16153189778503));
#4260=CARTESIAN_POINT('Ctrl Pts',(0.718829403428655,18.7531999223435,2.39509372919035));
#4261=CARTESIAN_POINT('Ctrl Pts',(-0.0593837235092117,18.8781999223435,
2.62865556059567));
#4262=CARTESIAN_POINT('Ctrl Pts',(-0.826255568446083,19.0031999223435,2.36018885228542));
#4263=CARTESIAN_POINT('Ctrl Pts',(-1.59312741338295,19.1281999223435,2.09172214397517));
#4264=CARTESIAN_POINT('Ctrl Pts',(-2.05573899656828,19.2531999223435,1.42377205367607));
#4265=CARTESIAN_POINT('Ctrl Pts',(-2.51835057975361,19.3781999223435,0.755821963376961));
#4266=CARTESIAN_POINT('Ctrl Pts',(-2.5,19.5031999223435,-0.056477277205306));
#4267=CARTESIAN_POINT('Ctrl Pts',(-2.48164942024639,19.6281999223435,-0.868776517787572));
#4268=CARTESIAN_POINT('Ctrl Pts',(-1.98934597530646,19.7531999223435,-1.5151542077863));
#4269=CARTESIAN_POINT('Ctrl Pts',(-1.49704253036652,19.8781999223435,-2.16153189778503));
#4270=CARTESIAN_POINT('Ctrl Pts',(-0.718829403428655,20.0031999223435,-2.39509372919035));
#4271=CARTESIAN_POINT('Ctrl Pts',(0.0593837235092121,20.1281999223436,-2.62865556059567));
#4272=CARTESIAN_POINT('Ctrl Pts',(0.826255568446083,20.2531999223435,-2.36018885228542));
#4273=CARTESIAN_POINT('Ctrl Pts',(1.59312741338295,20.3781999223435,-2.09172214397517));
#4274=CARTESIAN_POINT('Ctrl Pts',(2.05573899656828,20.5031999223436,-1.42377205367607));
#4275=CARTESIAN_POINT('Ctrl Pts',(2.51835057975361,20.6281999223435,-0.755821963376961));
#4276=CARTESIAN_POINT('Ctrl Pts',(2.5,20.7531999223436,0.0564772772053057));
#4277=CARTESIAN_POINT('Ctrl Pts',(2.48164942024639,20.8781999223436,0.868776517787572));
#4278=CARTESIAN_POINT('Ctrl Pts',(1.98934597530646,21.0031999223435,1.5151542077863));
#4279=CARTESIAN_POINT('Ctrl Pts',(1.49704253036652,21.1281999223435,2.16153189778503));
#4280=CARTESIAN_POINT('Ctrl Pts',(0.718829403428655,21.2531999223435,2.39509372919035));
#4281=CARTESIAN_POINT('Ctrl Pts',(-0.0593837235092117,21.3781999223435,
2.62865556059567));
#4282=CARTESIAN_POINT('Ctrl Pts',(-0.826255568446083,21.5031999223435,2.36018885228542));
#4283=CARTESIAN_POINT('Ctrl Pts',(-1.59312741338295,21.6281999223435,2.09172214397517));
#4284=CARTESIAN_POINT('Ctrl Pts',(-2.05573899656828,21.7531999223435,1.42377205367607));
#4285=CARTESIAN_POINT('Ctrl Pts',(-2.51835057975361,21.8781999223435,0.755821963376961));
#4286=CARTESIAN_POINT('Ctrl Pts',(-2.5,22.0031999223436,-0.056477277205306));
#4287=CARTESIAN_POINT('Ctrl Pts',(-2.48164942024639,22.1281999223435,-0.868776517787572));
#4288=CARTESIAN_POINT('Ctrl Pts',(-1.98934597530646,22.2531999223435,-1.5151542077863));
#4289=CARTESIAN_POINT('Ctrl Pts',(-1.49704253036652,22.3781999223435,-2.16153189778503));
#4290=CARTESIAN_POINT('Ctrl Pts',(-0.718829403428655,22.5031999223435,-2.39509372919035));
#4291=CARTESIAN_POINT('Ctrl Pts',(0.0593837235092121,22.6281999223436,-2.62865556059567));
#4292=CARTESIAN_POINT('Ctrl Pts',(0.826255568446083,22.7531999223435,-2.36018885228542));
#4293=CARTESIAN_POINT('Ctrl Pts',(1.59312741338295,22.8781999223435,-2.09172214397517));
#4294=CARTESIAN_POINT('Ctrl Pts',(2.05573899656828,23.0031999223435,-1.42377205367607));
#4295=CARTESIAN_POINT('Ctrl Pts',(2.51835057975361,23.1281999223435,-0.755821963376961));
#4296=CARTESIAN_POINT('Ctrl Pts',(2.5,23.2531999223436,0.0564772772053057));
#4297=CARTESIAN_POINT('Ctrl Pts',(2.48164942024639,23.3781999223435,0.868776517787572));
#4298=CARTESIAN_POINT('Ctrl Pts',(1.98934597530646,23.5031999223436,1.5151542077863));
#4299=CARTESIAN_POINT('Ctrl Pts',(1.49704253036652,23.6281999223435,2.16153189778503));
#4300=CARTESIAN_POINT('Ctrl Pts',(0.718829403428655,23.7531999223435,2.39509372919035));
#4301=CARTESIAN_POINT('Ctrl Pts',(-0.0593837235092117,23.8781999223435,
2.62865556059567));
#4302=CARTESIAN_POINT('Ctrl Pts',(-0.826255568446083,24.0031999223435,2.36018885228542));
#4303=CARTESIAN_POINT('Ctrl Pts',(-1.59312741338295,24.1281999223435,2.09172214397517));
#4304=CARTESIAN_POINT('Ctrl Pts',(-2.05573899656828,24.2531999223435,1.42377205367607));
#4305=CARTESIAN_POINT('Ctrl Pts',(-2.51835057975361,24.3781999223435,0.755821963376961));
#4306=CARTESIAN_POINT('Ctrl Pts',(-2.5,24.5031999223436,-0.056477277205306));
#4307=CARTESIAN_POINT('Ctrl Pts',(-2.48164942024639,24.6281999223435,-0.868776517787572));
#4308=CARTESIAN_POINT('Ctrl Pts',(-1.98934597530646,24.7531999223435,-1.5151542077863));
#4309=CARTESIAN_POINT('Ctrl Pts',(-1.49704253036652,24.8781999223436,-2.16153189778503));
#4310=CARTESIAN_POINT('Ctrl Pts',(-0.718829403428655,25.0031999223435,-2.39509372919035));
#4311=CARTESIAN_POINT('Ctrl Pts',(0.0593837235092121,25.1281999223435,-2.62865556059567));
#4312=CARTESIAN_POINT('Ctrl Pts',(0.826255568446083,25.2531999223435,-2.36018885228542));
#4313=CARTESIAN_POINT('Ctrl Pts',(1.59312741338295,25.3781999223435,-2.09172214397517));
#4314=CARTESIAN_POINT('Ctrl Pts',(2.05573899656828,25.5031999223435,-1.42377205367607));
#4315=CARTESIAN_POINT('Ctrl Pts',(2.51835057975361,25.6281999223435,-0.755821963376961));
#4316=CARTESIAN_POINT('Ctrl Pts',(2.5,25.7531999223436,0.0564772772053057));
#4317=CARTESIAN_POINT('Ctrl Pts',(2.48164942024639,25.8781999223436,0.868776517787572));
#4318=CARTESIAN_POINT('Ctrl Pts',(1.98934597530646,26.0031999223435,1.5151542077863));
#4319=CARTESIAN_POINT('Ctrl Pts',(1.49704253036652,26.1281999223435,2.16153189778503));
#4320=CARTESIAN_POINT('Ctrl Pts',(0.718829403428655,26.2531999223435,2.39509372919035));
#4321=CARTESIAN_POINT('Ctrl Pts',(-0.0593837235092117,26.3781999223436,
2.62865556059567));
#4322=CARTESIAN_POINT('Ctrl Pts',(-0.826255568446083,26.5031999223435,2.36018885228542));
#4323=CARTESIAN_POINT('Ctrl Pts',(-1.59312741338295,26.6281999223435,2.09172214397517));
#4324=CARTESIAN_POINT('Ctrl Pts',(-2.05573899656828,26.7531999223436,1.42377205367607));
#4325=CARTESIAN_POINT('Ctrl Pts',(-2.51835057975361,26.8781999223435,0.755821963376961));
#4326=CARTESIAN_POINT('Ctrl Pts',(-2.5,27.0031999223436,-0.056477277205306));
#4327=CARTESIAN_POINT('Ctrl Pts',(-2.48164942024639,27.1281999223436,-0.868776517787572));
#4328=CARTESIAN_POINT('Ctrl Pts',(-1.98934597530646,27.2531999223435,-1.5151542077863));
#4329=CARTESIAN_POINT('Ctrl Pts',(-1.49704253036652,27.3781999223436,-2.16153189778503));
#4330=CARTESIAN_POINT('Ctrl Pts',(-0.718829403428655,27.5031999223435,-2.39509372919035));
#4331=CARTESIAN_POINT('Ctrl Pts',(0.0593837235092121,27.6281999223435,-2.62865556059567));
#4332=CARTESIAN_POINT('Ctrl Pts',(0.826255568446083,27.7531999223436,-2.36018885228542));
#4333=CARTESIAN_POINT('Ctrl Pts',(1.59312741338295,27.8781999223436,-2.09172214397517));
#4334=CARTESIAN_POINT('Ctrl Pts',(2.05573899656828,28.0031999223436,-1.42377205367607));
#4335=CARTESIAN_POINT('Ctrl Pts',(2.51835057975361,28.1281999223436,-0.755821963376961));
#4336=CARTESIAN_POINT('Ctrl Pts',(2.5,28.2531999223436,0.0564772772053057));
#4337=CARTESIAN_POINT('Ctrl Pts',(2.48164942024639,28.3781999223436,0.868776517787572));
#4338=CARTESIAN_POINT('Ctrl Pts',(1.98934597530646,28.5031999223436,1.5151542077863));
#4339=CARTESIAN_POINT('Ctrl Pts',(1.49704253036652,28.6281999223436,2.16153189778503));
#4340=CARTESIAN_POINT('Ctrl Pts',(0.718829403428655,28.7531999223435,2.39509372919035));
#4341=CARTESIAN_POINT('Ctrl Pts',(-0.0593837235092117,28.8781999223435,
2.62865556059567));
#4342=CARTESIAN_POINT('Ctrl Pts',(-0.826255568446083,29.0031999223436,2.36018885228542));
#4343=CARTESIAN_POINT('Ctrl Pts',(-1.59312741338295,29.1281999223435,2.09172214397517));
#4344=CARTESIAN_POINT('Ctrl Pts',(-2.05573899656828,29.2531999223436,1.42377205367607));
#4345=CARTESIAN_POINT('Ctrl Pts',(-2.51835057975361,29.3781999223436,0.755821963376961));
#4346=CARTESIAN_POINT('Ctrl Pts',(-2.5,29.5031999223436,-0.056477277205306));
#4347=CARTESIAN_POINT('Ctrl Pts',(-2.48164942024639,29.6281999223435,-0.868776517787572));
#4348=CARTESIAN_POINT('Ctrl Pts',(-1.98934597530646,29.7531999223435,-1.5151542077863));
#4349=CARTESIAN_POINT('Ctrl Pts',(-1.49704253036652,29.8781999223435,-2.16153189778503));
#4350=CARTESIAN_POINT('Ctrl Pts',(-0.718829403428655,30.0031999223435,-2.39509372919035));
#4351=CARTESIAN_POINT('Ctrl Pts',(0.0593837235092121,30.1281999223435,-2.62865556059567));
#4352=CARTESIAN_POINT('Ctrl Pts',(0.826255568446083,30.2531999223435,-2.36018885228542));
#4353=CARTESIAN_POINT('Ctrl Pts',(1.59312741338295,30.3781999223435,-2.09172214397517));
#4354=CARTESIAN_POINT('Ctrl Pts',(2.05573899656828,30.5031999223436,-1.42377205367607));
#4355=CARTESIAN_POINT('Ctrl Pts',(2.51835057975361,30.6281999223436,-0.755821963376961));
#4356=CARTESIAN_POINT('Ctrl Pts',(2.5,30.7531999223435,0.0564772772053057));
#4357=CARTESIAN_POINT('Ctrl Pts',(2.48164942024639,30.8781999223435,0.868776517787572));
#4358=CARTESIAN_POINT('Ctrl Pts',(1.98934597530646,31.0031999223436,1.5151542077863));
#4359=CARTESIAN_POINT('Ctrl Pts',(1.49704253036652,31.1281999223435,2.16153189778503));
#4360=CARTESIAN_POINT('Ctrl Pts',(0.718829403428655,31.2531999223435,2.39509372919035));
#4361=CARTESIAN_POINT('Ctrl Pts',(-0.0593837235092117,31.3781999223435,
2.62865556059567));
#4362=CARTESIAN_POINT('Ctrl Pts',(-0.826255568446083,31.5031999223435,2.36018885228542));
#4363=CARTESIAN_POINT('Ctrl Pts',(-1.59312741338295,31.6281999223435,2.09172214397517));
#4364=CARTESIAN_POINT('Ctrl Pts',(-2.05573899656828,31.7531999223436,1.42377205367607));
#4365=CARTESIAN_POINT('Ctrl Pts',(-2.51835057975361,31.8781999223435,0.755821963376961));
#4366=CARTESIAN_POINT('Ctrl Pts',(-2.5,32.0031999223435,-0.056477277205306));
#4367=CARTESIAN_POINT('Ctrl Pts',(-2.48164942024639,32.1281999223435,-0.868776517787572));
#4368=CARTESIAN_POINT('Ctrl Pts',(-1.98934597530646,32.2531999223435,-1.5151542077863));
#4369=CARTESIAN_POINT('Ctrl Pts',(-1.49704253036652,32.3781999223435,-2.16153189778503));
#4370=CARTESIAN_POINT('Ctrl Pts',(-0.718829403428655,32.5031999223435,-2.39509372919035));
#4371=CARTESIAN_POINT('Ctrl Pts',(0.0593837235092121,32.6281999223435,-2.62865556059567));
#4372=CARTESIAN_POINT('Ctrl Pts',(0.826255568446083,32.7531999223435,-2.36018885228542));
#4373=CARTESIAN_POINT('Ctrl Pts',(1.59312741338295,32.8781999223435,-2.09172214397517));
#4374=CARTESIAN_POINT('Ctrl Pts',(2.05573899656828,33.0031999223436,-1.42377205367607));
#4375=CARTESIAN_POINT('Ctrl Pts',(2.51835057975361,33.1281999223435,-0.755821963376961));
#4376=CARTESIAN_POINT('Ctrl Pts',(2.5,33.2531999223435,0.0564772772053057));
#4377=CARTESIAN_POINT('Ctrl Pts',(2.48164942024639,33.3781999223435,0.868776517787572));
#4378=CARTESIAN_POINT('Ctrl Pts',(1.98934597530646,33.5031999223435,1.5151542077863));
#4379=CARTESIAN_POINT('Ctrl Pts',(1.49704253036652,33.6281999223436,2.16153189778503));
#4380=CARTESIAN_POINT('Ctrl Pts',(0.718829403428655,33.7531999223435,2.39509372919035));
#4381=CARTESIAN_POINT('Ctrl Pts',(-0.0593837235092117,33.8781999223435,
2.62865556059567));
#4382=CARTESIAN_POINT('Ctrl Pts',(-0.826255568446083,34.0031999223435,2.36018885228542));
#4383=CARTESIAN_POINT('Ctrl Pts',(-1.59312741338295,34.1281999223435,2.09172214397517));
#4384=CARTESIAN_POINT('Ctrl Pts',(-2.05573899656828,34.2531999223435,1.42377205367607));
#4385=CARTESIAN_POINT('Ctrl Pts',(-2.51835057975361,34.3781999223435,0.755821963376961));
#4386=CARTESIAN_POINT('Ctrl Pts',(-2.5,34.5031999223435,-0.056477277205306));
#4387=CARTESIAN_POINT('Ctrl Pts',(-2.48164942024639,34.6281999223435,-0.868776517787572));
#4388=CARTESIAN_POINT('Ctrl Pts',(-1.98934597530646,34.7531999223435,-1.5151542077863));
#4389=CARTESIAN_POINT('Ctrl Pts',(-1.49704253036652,34.8781999223436,-2.16153189778503));
#4390=CARTESIAN_POINT('Ctrl Pts',(-0.718829403428655,35.0031999223435,-2.39509372919035));
#4391=CARTESIAN_POINT('Ctrl Pts',(0.0593837235092121,35.1281999223435,-2.62865556059567));
#4392=CARTESIAN_POINT('Ctrl Pts',(0.826255568446083,35.2531999223435,-2.36018885228542));
#4393=CARTESIAN_POINT('Ctrl Pts',(1.59312741338295,35.3781999223435,-2.09172214397517));
#4394=CARTESIAN_POINT('Ctrl Pts',(2.05573899656828,35.5031999223436,-1.42377205367607));
#4395=CARTESIAN_POINT('Ctrl Pts',(2.51835057975361,35.6281999223435,-0.755821963376961));
#4396=CARTESIAN_POINT('Ctrl Pts',(2.5,35.7531999223435,0.0564772772053057));
#4397=CARTESIAN_POINT('Ctrl Pts',(2.48164942024639,35.8781999223435,0.868776517787572));
#4398=CARTESIAN_POINT('Ctrl Pts',(1.98934597530646,36.0031999223435,1.5151542077863));
#4399=CARTESIAN_POINT('Ctrl Pts',(1.49704253036652,36.1281999223436,2.16153189778503));
#4400=CARTESIAN_POINT('Ctrl Pts',(0.718829403428655,36.2531999223435,2.39509372919035));
#4401=CARTESIAN_POINT('Ctrl Pts',(-0.0593837235092117,36.3781999223435,
2.62865556059567));
#4402=CARTESIAN_POINT('Ctrl Pts',(-0.826255568446083,36.5031999223435,2.36018885228542));
#4403=CARTESIAN_POINT('Ctrl Pts',(-1.59312741338295,36.6281999223435,2.09172214397517));
#4404=CARTESIAN_POINT('Ctrl Pts',(-2.05573899656828,36.7531999223436,1.42377205367607));
#4405=CARTESIAN_POINT('Ctrl Pts',(-2.51835057975361,36.8781999223435,0.755821963376961));
#4406=CARTESIAN_POINT('Ctrl Pts',(-2.5,37.0031999223435,-0.056477277205306));
#4407=CARTESIAN_POINT('Ctrl Pts',(-2.48164942024639,37.1281999223435,-0.868776517787572));
#4408=CARTESIAN_POINT('Ctrl Pts',(-1.98934597530646,37.2531999223435,-1.5151542077863));
#4409=CARTESIAN_POINT('Ctrl Pts',(-1.49704253036652,37.3781999223436,-2.16153189778503));
#4410=CARTESIAN_POINT('Ctrl Pts',(-0.718829403428655,37.5031999223435,-2.39509372919035));
#4411=CARTESIAN_POINT('Ctrl Pts',(0.0593837235092121,37.6281999223435,-2.62865556059567));
#4412=CARTESIAN_POINT('Ctrl Pts',(0.826255568446083,37.7531999223435,-2.36018885228542));
#4413=CARTESIAN_POINT('Ctrl Pts',(1.59312741338295,37.8781999223435,-2.09172214397517));
#4414=CARTESIAN_POINT('Ctrl Pts',(2.05573899656828,38.0031999223435,-1.42377205367607));
#4415=CARTESIAN_POINT('Ctrl Pts',(2.51835057975361,38.1281999223435,-0.755821963376961));
#4416=CARTESIAN_POINT('Ctrl Pts',(2.5,38.2531999223435,0.0564772772053057));
#4417=CARTESIAN_POINT('Ctrl Pts',(2.48164942024639,38.3781999223435,0.868776517787572));
#4418=CARTESIAN_POINT('Ctrl Pts',(1.98934597530646,38.5031999223435,1.5151542077863));
#4419=CARTESIAN_POINT('Ctrl Pts',(1.49704253036652,38.6281999223436,2.16153189778503));
#4420=CARTESIAN_POINT('Ctrl Pts',(0.718829403428655,38.7531999223435,2.39509372919035));
#4421=CARTESIAN_POINT('Ctrl Pts',(-0.0593837235092117,38.8781999223435,
2.62865556059567));
#4422=CARTESIAN_POINT('Ctrl Pts',(-0.826255568446083,39.0031999223436,2.36018885228542));
#4423=CARTESIAN_POINT('Ctrl Pts',(-1.59312741338295,39.1281999223435,2.09172214397517));
#4424=CARTESIAN_POINT('Ctrl Pts',(-2.05573899656828,39.2531999223436,1.42377205367607));
#4425=CARTESIAN_POINT('Ctrl Pts',(-2.51835057975361,39.3781999223435,0.755821963376961));
#4426=CARTESIAN_POINT('Ctrl Pts',(-2.5,39.5031999223436,-0.056477277205306));
#4427=CARTESIAN_POINT('Ctrl Pts',(-3.5,14.5031999223435,-0.0564772772052956));
#4428=CARTESIAN_POINT('Ctrl Pts',(-3.48164942024639,14.6281999223435,-1.19369621402047));
#4429=CARTESIAN_POINT('Ctrl Pts',(-2.79836296968141,14.7531999223435,-2.10293946007877));
#4430=CARTESIAN_POINT('Ctrl Pts',(-2.11507651911643,14.8781999223435,-3.01218270613706));
#4431=CARTESIAN_POINT('Ctrl Pts',(-1.02784639780361,15.0031999223435,-3.3461502454855));
#4432=CARTESIAN_POINT('Ctrl Pts',(0.0593837235092011,15.1281999223435,-3.68011778483394));
#4433=CARTESIAN_POINT('Ctrl Pts',(1.13527256282102,15.2531999223435,-3.31124536858058));
#4434=CARTESIAN_POINT('Ctrl Pts',(2.21116140213284,15.3781999223435,-2.94237295232722));
#4435=CARTESIAN_POINT('Ctrl Pts',(2.86475599094322,15.5031999223435,-2.01155730596855));
#4436=CARTESIAN_POINT('Ctrl Pts',(3.51835057975361,15.6281999223435,-1.08074165960988));
#4437=CARTESIAN_POINT('Ctrl Pts',(3.5,15.7531999223435,0.0564772772052952));
#4438=CARTESIAN_POINT('Ctrl Pts',(3.48164942024639,15.8781999223435,1.19369621402047));
#4439=CARTESIAN_POINT('Ctrl Pts',(2.79836296968141,16.0031999223435,2.10293946007876));
#4440=CARTESIAN_POINT('Ctrl Pts',(2.11507651911643,16.1281999223435,3.01218270613706));
#4441=CARTESIAN_POINT('Ctrl Pts',(1.02784639780361,16.2531999223435,3.3461502454855));
#4442=CARTESIAN_POINT('Ctrl Pts',(-0.0593837235092006,16.3781999223435,
3.68011778483394));
#4443=CARTESIAN_POINT('Ctrl Pts',(-1.13527256282102,16.5031999223435,3.31124536858058));
#4444=CARTESIAN_POINT('Ctrl Pts',(-2.21116140213284,16.6281999223435,2.94237295232722));
#4445=CARTESIAN_POINT('Ctrl Pts',(-2.86475599094322,16.7531999223435,2.01155730596855));
#4446=CARTESIAN_POINT('Ctrl Pts',(-3.51835057975361,16.8781999223435,1.08074165960988));
#4447=CARTESIAN_POINT('Ctrl Pts',(-3.5,17.0031999223435,-0.0564772772052956));
#4448=CARTESIAN_POINT('Ctrl Pts',(-3.48164942024639,17.1281999223435,-1.19369621402047));
#4449=CARTESIAN_POINT('Ctrl Pts',(-2.79836296968141,17.2531999223435,-2.10293946007877));
#4450=CARTESIAN_POINT('Ctrl Pts',(-2.11507651911643,17.3781999223435,-3.01218270613706));
#4451=CARTESIAN_POINT('Ctrl Pts',(-1.02784639780361,17.5031999223435,-3.3461502454855));
#4452=CARTESIAN_POINT('Ctrl Pts',(0.0593837235092011,17.6281999223435,-3.68011778483394));
#4453=CARTESIAN_POINT('Ctrl Pts',(1.13527256282102,17.7531999223435,-3.31124536858058));
#4454=CARTESIAN_POINT('Ctrl Pts',(2.21116140213284,17.8781999223435,-2.94237295232722));
#4455=CARTESIAN_POINT('Ctrl Pts',(2.86475599094322,18.0031999223435,-2.01155730596855));
#4456=CARTESIAN_POINT('Ctrl Pts',(3.51835057975361,18.1281999223435,-1.08074165960988));
#4457=CARTESIAN_POINT('Ctrl Pts',(3.5,18.2531999223435,0.0564772772052952));
#4458=CARTESIAN_POINT('Ctrl Pts',(3.48164942024639,18.3781999223435,1.19369621402047));
#4459=CARTESIAN_POINT('Ctrl Pts',(2.79836296968141,18.5031999223435,2.10293946007876));
#4460=CARTESIAN_POINT('Ctrl Pts',(2.11507651911643,18.6281999223435,3.01218270613706));
#4461=CARTESIAN_POINT('Ctrl Pts',(1.02784639780361,18.7531999223435,3.3461502454855));
#4462=CARTESIAN_POINT('Ctrl Pts',(-0.0593837235092006,18.8781999223435,
3.68011778483394));
#4463=CARTESIAN_POINT('Ctrl Pts',(-1.13527256282102,19.0031999223435,3.31124536858058));
#4464=CARTESIAN_POINT('Ctrl Pts',(-2.21116140213284,19.1281999223435,2.94237295232722));
#4465=CARTESIAN_POINT('Ctrl Pts',(-2.86475599094322,19.2531999223435,2.01155730596855));
#4466=CARTESIAN_POINT('Ctrl Pts',(-3.51835057975361,19.3781999223435,1.08074165960988));
#4467=CARTESIAN_POINT('Ctrl Pts',(-3.5,19.5031999223435,-0.0564772772052956));
#4468=CARTESIAN_POINT('Ctrl Pts',(-3.48164942024639,19.6281999223435,-1.19369621402047));
#4469=CARTESIAN_POINT('Ctrl Pts',(-2.79836296968141,19.7531999223435,-2.10293946007877));
#4470=CARTESIAN_POINT('Ctrl Pts',(-2.11507651911643,19.8781999223435,-3.01218270613706));
#4471=CARTESIAN_POINT('Ctrl Pts',(-1.02784639780361,20.0031999223435,-3.3461502454855));
#4472=CARTESIAN_POINT('Ctrl Pts',(0.0593837235092011,20.1281999223435,-3.68011778483394));
#4473=CARTESIAN_POINT('Ctrl Pts',(1.13527256282102,20.2531999223435,-3.31124536858058));
#4474=CARTESIAN_POINT('Ctrl Pts',(2.21116140213284,20.3781999223435,-2.94237295232722));
#4475=CARTESIAN_POINT('Ctrl Pts',(2.86475599094322,20.5031999223435,-2.01155730596855));
#4476=CARTESIAN_POINT('Ctrl Pts',(3.51835057975361,20.6281999223435,-1.08074165960988));
#4477=CARTESIAN_POINT('Ctrl Pts',(3.5,20.7531999223435,0.0564772772052952));
#4478=CARTESIAN_POINT('Ctrl Pts',(3.48164942024639,20.8781999223435,1.19369621402047));
#4479=CARTESIAN_POINT('Ctrl Pts',(2.79836296968141,21.0031999223435,2.10293946007876));
#4480=CARTESIAN_POINT('Ctrl Pts',(2.11507651911643,21.1281999223435,3.01218270613706));
#4481=CARTESIAN_POINT('Ctrl Pts',(1.02784639780361,21.2531999223435,3.3461502454855));
#4482=CARTESIAN_POINT('Ctrl Pts',(-0.0593837235092006,21.3781999223435,
3.68011778483394));
#4483=CARTESIAN_POINT('Ctrl Pts',(-1.13527256282102,21.5031999223435,3.31124536858058));
#4484=CARTESIAN_POINT('Ctrl Pts',(-2.21116140213284,21.6281999223435,2.94237295232722));
#4485=CARTESIAN_POINT('Ctrl Pts',(-2.86475599094322,21.7531999223435,2.01155730596855));
#4486=CARTESIAN_POINT('Ctrl Pts',(-3.51835057975361,21.8781999223435,1.08074165960988));
#4487=CARTESIAN_POINT('Ctrl Pts',(-3.5,22.0031999223435,-0.0564772772052956));
#4488=CARTESIAN_POINT('Ctrl Pts',(-3.48164942024639,22.1281999223435,-1.19369621402047));
#4489=CARTESIAN_POINT('Ctrl Pts',(-2.79836296968141,22.2531999223435,-2.10293946007877));
#4490=CARTESIAN_POINT('Ctrl Pts',(-2.11507651911643,22.3781999223435,-3.01218270613706));
#4491=CARTESIAN_POINT('Ctrl Pts',(-1.02784639780361,22.5031999223435,-3.3461502454855));
#4492=CARTESIAN_POINT('Ctrl Pts',(0.0593837235092011,22.6281999223435,-3.68011778483394));
#4493=CARTESIAN_POINT('Ctrl Pts',(1.13527256282102,22.7531999223435,-3.31124536858058));
#4494=CARTESIAN_POINT('Ctrl Pts',(2.21116140213284,22.8781999223435,-2.94237295232722));
#4495=CARTESIAN_POINT('Ctrl Pts',(2.86475599094322,23.0031999223435,-2.01155730596855));
#4496=CARTESIAN_POINT('Ctrl Pts',(3.51835057975361,23.1281999223435,-1.08074165960988));
#4497=CARTESIAN_POINT('Ctrl Pts',(3.5,23.2531999223435,0.0564772772052952));
#4498=CARTESIAN_POINT('Ctrl Pts',(3.48164942024639,23.3781999223435,1.19369621402047));
#4499=CARTESIAN_POINT('Ctrl Pts',(2.79836296968141,23.5031999223435,2.10293946007876));
#4500=CARTESIAN_POINT('Ctrl Pts',(2.11507651911643,23.6281999223435,3.01218270613706));
#4501=CARTESIAN_POINT('Ctrl Pts',(1.02784639780361,23.7531999223435,3.3461502454855));
#4502=CARTESIAN_POINT('Ctrl Pts',(-0.0593837235092006,23.8781999223435,
3.68011778483394));
#4503=CARTESIAN_POINT('Ctrl Pts',(-1.13527256282102,24.0031999223435,3.31124536858058));
#4504=CARTESIAN_POINT('Ctrl Pts',(-2.21116140213284,24.1281999223435,2.94237295232722));
#4505=CARTESIAN_POINT('Ctrl Pts',(-2.86475599094322,24.2531999223435,2.01155730596855));
#4506=CARTESIAN_POINT('Ctrl Pts',(-3.51835057975361,24.3781999223435,1.08074165960988));
#4507=CARTESIAN_POINT('Ctrl Pts',(-3.5,24.5031999223435,-0.0564772772052956));
#4508=CARTESIAN_POINT('Ctrl Pts',(-3.48164942024639,24.6281999223435,-1.19369621402047));
#4509=CARTESIAN_POINT('Ctrl Pts',(-2.79836296968141,24.7531999223435,-2.10293946007877));
#4510=CARTESIAN_POINT('Ctrl Pts',(-2.11507651911643,24.8781999223436,-3.01218270613706));
#4511=CARTESIAN_POINT('Ctrl Pts',(-1.02784639780361,25.0031999223435,-3.3461502454855));
#4512=CARTESIAN_POINT('Ctrl Pts',(0.0593837235092011,25.1281999223435,-3.68011778483394));
#4513=CARTESIAN_POINT('Ctrl Pts',(1.13527256282102,25.2531999223435,-3.31124536858058));
#4514=CARTESIAN_POINT('Ctrl Pts',(2.21116140213284,25.3781999223435,-2.94237295232722));
#4515=CARTESIAN_POINT('Ctrl Pts',(2.86475599094322,25.5031999223436,-2.01155730596855));
#4516=CARTESIAN_POINT('Ctrl Pts',(3.51835057975361,25.6281999223435,-1.08074165960988));
#4517=CARTESIAN_POINT('Ctrl Pts',(3.5,25.7531999223436,0.0564772772052952));
#4518=CARTESIAN_POINT('Ctrl Pts',(3.48164942024639,25.8781999223435,1.19369621402047));
#4519=CARTESIAN_POINT('Ctrl Pts',(2.79836296968141,26.0031999223435,2.10293946007876));
#4520=CARTESIAN_POINT('Ctrl Pts',(2.11507651911643,26.1281999223436,3.01218270613706));
#4521=CARTESIAN_POINT('Ctrl Pts',(1.02784639780361,26.2531999223435,3.3461502454855));
#4522=CARTESIAN_POINT('Ctrl Pts',(-0.0593837235092006,26.3781999223435,
3.68011778483394));
#4523=CARTESIAN_POINT('Ctrl Pts',(-1.13527256282102,26.5031999223435,3.31124536858058));
#4524=CARTESIAN_POINT('Ctrl Pts',(-2.21116140213284,26.6281999223435,2.94237295232722));
#4525=CARTESIAN_POINT('Ctrl Pts',(-2.86475599094322,26.7531999223436,2.01155730596855));
#4526=CARTESIAN_POINT('Ctrl Pts',(-3.51835057975361,26.8781999223435,1.08074165960988));
#4527=CARTESIAN_POINT('Ctrl Pts',(-3.5,27.0031999223436,-0.0564772772052956));
#4528=CARTESIAN_POINT('Ctrl Pts',(-3.48164942024639,27.1281999223435,-1.19369621402047));
#4529=CARTESIAN_POINT('Ctrl Pts',(-2.79836296968141,27.2531999223435,-2.10293946007877));
#4530=CARTESIAN_POINT('Ctrl Pts',(-2.11507651911643,27.3781999223436,-3.01218270613706));
#4531=CARTESIAN_POINT('Ctrl Pts',(-1.02784639780361,27.5031999223435,-3.3461502454855));
#4532=CARTESIAN_POINT('Ctrl Pts',(0.0593837235092011,27.6281999223435,-3.68011778483394));
#4533=CARTESIAN_POINT('Ctrl Pts',(1.13527256282102,27.7531999223435,-3.31124536858058));
#4534=CARTESIAN_POINT('Ctrl Pts',(2.21116140213284,27.8781999223435,-2.94237295232722));
#4535=CARTESIAN_POINT('Ctrl Pts',(2.86475599094322,28.0031999223435,-2.01155730596855));
#4536=CARTESIAN_POINT('Ctrl Pts',(3.51835057975361,28.1281999223435,-1.08074165960988));
#4537=CARTESIAN_POINT('Ctrl Pts',(3.5,28.2531999223435,0.0564772772052952));
#4538=CARTESIAN_POINT('Ctrl Pts',(3.48164942024639,28.3781999223435,1.19369621402047));
#4539=CARTESIAN_POINT('Ctrl Pts',(2.79836296968141,28.5031999223435,2.10293946007876));
#4540=CARTESIAN_POINT('Ctrl Pts',(2.11507651911643,28.6281999223435,3.01218270613706));
#4541=CARTESIAN_POINT('Ctrl Pts',(1.02784639780361,28.7531999223435,3.3461502454855));
#4542=CARTESIAN_POINT('Ctrl Pts',(-0.0593837235092006,28.8781999223435,
3.68011778483394));
#4543=CARTESIAN_POINT('Ctrl Pts',(-1.13527256282102,29.0031999223435,3.31124536858058));
#4544=CARTESIAN_POINT('Ctrl Pts',(-2.21116140213284,29.1281999223435,2.94237295232722));
#4545=CARTESIAN_POINT('Ctrl Pts',(-2.86475599094322,29.2531999223435,2.01155730596855));
#4546=CARTESIAN_POINT('Ctrl Pts',(-3.51835057975361,29.3781999223435,1.08074165960988));
#4547=CARTESIAN_POINT('Ctrl Pts',(-3.5,29.5031999223435,-0.0564772772052956));
#4548=CARTESIAN_POINT('Ctrl Pts',(-3.48164942024639,29.6281999223435,-1.19369621402047));
#4549=CARTESIAN_POINT('Ctrl Pts',(-2.79836296968141,29.7531999223435,-2.10293946007877));
#4550=CARTESIAN_POINT('Ctrl Pts',(-2.11507651911643,29.8781999223435,-3.01218270613706));
#4551=CARTESIAN_POINT('Ctrl Pts',(-1.02784639780361,30.0031999223435,-3.3461502454855));
#4552=CARTESIAN_POINT('Ctrl Pts',(0.0593837235092011,30.1281999223435,-3.68011778483394));
#4553=CARTESIAN_POINT('Ctrl Pts',(1.13527256282102,30.2531999223435,-3.31124536858058));
#4554=CARTESIAN_POINT('Ctrl Pts',(2.21116140213284,30.3781999223435,-2.94237295232722));
#4555=CARTESIAN_POINT('Ctrl Pts',(2.86475599094322,30.5031999223435,-2.01155730596855));
#4556=CARTESIAN_POINT('Ctrl Pts',(3.51835057975361,30.6281999223435,-1.08074165960988));
#4557=CARTESIAN_POINT('Ctrl Pts',(3.5,30.7531999223435,0.0564772772052952));
#4558=CARTESIAN_POINT('Ctrl Pts',(3.48164942024639,30.8781999223435,1.19369621402047));
#4559=CARTESIAN_POINT('Ctrl Pts',(2.79836296968141,31.0031999223435,2.10293946007876));
#4560=CARTESIAN_POINT('Ctrl Pts',(2.11507651911643,31.1281999223435,3.01218270613706));
#4561=CARTESIAN_POINT('Ctrl Pts',(1.02784639780361,31.2531999223435,3.3461502454855));
#4562=CARTESIAN_POINT('Ctrl Pts',(-0.0593837235092006,31.3781999223435,
3.68011778483394));
#4563=CARTESIAN_POINT('Ctrl Pts',(-1.13527256282102,31.5031999223435,3.31124536858058));
#4564=CARTESIAN_POINT('Ctrl Pts',(-2.21116140213284,31.6281999223435,2.94237295232722));
#4565=CARTESIAN_POINT('Ctrl Pts',(-2.86475599094322,31.7531999223435,2.01155730596855));
#4566=CARTESIAN_POINT('Ctrl Pts',(-3.51835057975361,31.8781999223435,1.08074165960988));
#4567=CARTESIAN_POINT('Ctrl Pts',(-3.5,32.0031999223435,-0.0564772772052956));
#4568=CARTESIAN_POINT('Ctrl Pts',(-3.48164942024639,32.1281999223435,-1.19369621402047));
#4569=CARTESIAN_POINT('Ctrl Pts',(-2.79836296968141,32.2531999223435,-2.10293946007877));
#4570=CARTESIAN_POINT('Ctrl Pts',(-2.11507651911643,32.3781999223436,-3.01218270613706));
#4571=CARTESIAN_POINT('Ctrl Pts',(-1.02784639780361,32.5031999223435,-3.3461502454855));
#4572=CARTESIAN_POINT('Ctrl Pts',(0.0593837235092011,32.6281999223435,-3.68011778483394));
#4573=CARTESIAN_POINT('Ctrl Pts',(1.13527256282102,32.7531999223435,-3.31124536858058));
#4574=CARTESIAN_POINT('Ctrl Pts',(2.21116140213284,32.8781999223435,-2.94237295232722));
#4575=CARTESIAN_POINT('Ctrl Pts',(2.86475599094322,33.0031999223436,-2.01155730596855));
#4576=CARTESIAN_POINT('Ctrl Pts',(3.51835057975361,33.1281999223435,-1.08074165960988));
#4577=CARTESIAN_POINT('Ctrl Pts',(3.5,33.2531999223435,0.0564772772052952));
#4578=CARTESIAN_POINT('Ctrl Pts',(3.48164942024639,33.3781999223435,1.19369621402047));
#4579=CARTESIAN_POINT('Ctrl Pts',(2.79836296968141,33.5031999223435,2.10293946007876));
#4580=CARTESIAN_POINT('Ctrl Pts',(2.11507651911643,33.6281999223435,3.01218270613706));
#4581=CARTESIAN_POINT('Ctrl Pts',(1.02784639780361,33.7531999223435,3.3461502454855));
#4582=CARTESIAN_POINT('Ctrl Pts',(-0.0593837235092006,33.8781999223435,
3.68011778483394));
#4583=CARTESIAN_POINT('Ctrl Pts',(-1.13527256282102,34.0031999223435,3.31124536858058));
#4584=CARTESIAN_POINT('Ctrl Pts',(-2.21116140213284,34.1281999223436,2.94237295232722));
#4585=CARTESIAN_POINT('Ctrl Pts',(-2.86475599094322,34.2531999223436,2.01155730596855));
#4586=CARTESIAN_POINT('Ctrl Pts',(-3.51835057975361,34.3781999223435,1.08074165960988));
#4587=CARTESIAN_POINT('Ctrl Pts',(-3.5,34.5031999223435,-0.0564772772052956));
#4588=CARTESIAN_POINT('Ctrl Pts',(-3.48164942024639,34.6281999223435,-1.19369621402047));
#4589=CARTESIAN_POINT('Ctrl Pts',(-2.79836296968141,34.7531999223435,-2.10293946007877));
#4590=CARTESIAN_POINT('Ctrl Pts',(-2.11507651911643,34.8781999223436,-3.01218270613706));
#4591=CARTESIAN_POINT('Ctrl Pts',(-1.02784639780361,35.0031999223435,-3.3461502454855));
#4592=CARTESIAN_POINT('Ctrl Pts',(0.0593837235092011,35.1281999223435,-3.68011778483394));
#4593=CARTESIAN_POINT('Ctrl Pts',(1.13527256282102,35.2531999223435,-3.31124536858058));
#4594=CARTESIAN_POINT('Ctrl Pts',(2.21116140213284,35.3781999223435,-2.94237295232722));
#4595=CARTESIAN_POINT('Ctrl Pts',(2.86475599094322,35.5031999223436,-2.01155730596855));
#4596=CARTESIAN_POINT('Ctrl Pts',(3.51835057975361,35.6281999223435,-1.08074165960988));
#4597=CARTESIAN_POINT('Ctrl Pts',(3.5,35.7531999223435,0.0564772772052952));
#4598=CARTESIAN_POINT('Ctrl Pts',(3.48164942024639,35.8781999223435,1.19369621402047));
#4599=CARTESIAN_POINT('Ctrl Pts',(2.79836296968141,36.0031999223435,2.10293946007876));
#4600=CARTESIAN_POINT('Ctrl Pts',(2.11507651911643,36.1281999223436,3.01218270613706));
#4601=CARTESIAN_POINT('Ctrl Pts',(1.02784639780361,36.2531999223435,3.3461502454855));
#4602=CARTESIAN_POINT('Ctrl Pts',(-0.0593837235092006,36.3781999223436,
3.68011778483394));
#4603=CARTESIAN_POINT('Ctrl Pts',(-1.13527256282102,36.5031999223435,3.31124536858058));
#4604=CARTESIAN_POINT('Ctrl Pts',(-2.21116140213284,36.6281999223435,2.94237295232722));
#4605=CARTESIAN_POINT('Ctrl Pts',(-2.86475599094322,36.7531999223435,2.01155730596855));
#4606=CARTESIAN_POINT('Ctrl Pts',(-3.51835057975361,36.8781999223435,1.08074165960988));
#4607=CARTESIAN_POINT('Ctrl Pts',(-3.5,37.0031999223435,-0.0564772772052956));
#4608=CARTESIAN_POINT('Ctrl Pts',(-3.48164942024639,37.1281999223435,-1.19369621402047));
#4609=CARTESIAN_POINT('Ctrl Pts',(-2.79836296968141,37.2531999223435,-2.10293946007877));
#4610=CARTESIAN_POINT('Ctrl Pts',(-2.11507651911643,37.3781999223435,-3.01218270613706));
#4611=CARTESIAN_POINT('Ctrl Pts',(-1.02784639780361,37.5031999223435,-3.3461502454855));
#4612=CARTESIAN_POINT('Ctrl Pts',(0.0593837235092011,37.6281999223435,-3.68011778483394));
#4613=CARTESIAN_POINT('Ctrl Pts',(1.13527256282102,37.7531999223435,-3.31124536858058));
#4614=CARTESIAN_POINT('Ctrl Pts',(2.21116140213284,37.8781999223435,-2.94237295232722));
#4615=CARTESIAN_POINT('Ctrl Pts',(2.86475599094322,38.0031999223435,-2.01155730596855));
#4616=CARTESIAN_POINT('Ctrl Pts',(3.51835057975361,38.1281999223435,-1.08074165960988));
#4617=CARTESIAN_POINT('Ctrl Pts',(3.5,38.2531999223435,0.0564772772052952));
#4618=CARTESIAN_POINT('Ctrl Pts',(3.48164942024639,38.3781999223435,1.19369621402047));
#4619=CARTESIAN_POINT('Ctrl Pts',(2.79836296968141,38.5031999223435,2.10293946007876));
#4620=CARTESIAN_POINT('Ctrl Pts',(2.11507651911643,38.6281999223436,3.01218270613706));
#4621=CARTESIAN_POINT('Ctrl Pts',(1.02784639780361,38.7531999223435,3.3461502454855));
#4622=CARTESIAN_POINT('Ctrl Pts',(-0.0593837235092006,38.8781999223435,
3.68011778483394));
#4623=CARTESIAN_POINT('Ctrl Pts',(-1.13527256282102,39.0031999223435,3.31124536858058));
#4624=CARTESIAN_POINT('Ctrl Pts',(-2.21116140213284,39.1281999223435,2.94237295232722));
#4625=CARTESIAN_POINT('Ctrl Pts',(-2.86475599094322,39.2531999223436,2.01155730596855));
#4626=CARTESIAN_POINT('Ctrl Pts',(-3.51835057975361,39.3781999223435,1.08074165960988));
#4627=CARTESIAN_POINT('Ctrl Pts',(-3.5,39.5031999223435,-0.0564772772052956));
#4628=CARTESIAN_POINT('Ctrl Pts',(-4.5,14.5031999223435,-0.0564772772052853));
#4629=CARTESIAN_POINT('Ctrl Pts',(-4.4816494202464,14.6281999223435,-1.51861591025336));
#4630=CARTESIAN_POINT('Ctrl Pts',(-3.60737996405636,14.7531999223435,-2.69072471237123));
#4631=CARTESIAN_POINT('Ctrl Pts',(-2.73311050786633,14.8781999223435,-3.8628335144891));
#4632=CARTESIAN_POINT('Ctrl Pts',(-1.33686339217857,15.0031999223435,-4.29720676178065));
#4633=CARTESIAN_POINT('Ctrl Pts',(0.0593837235091902,15.1281999223435,-4.7315800090722));
#4634=CARTESIAN_POINT('Ctrl Pts',(1.44428955719596,15.2531999223435,-4.26230188487573));
#4635=CARTESIAN_POINT('Ctrl Pts',(2.82919539088272,15.3781999223435,-3.79302376067926));
#4636=CARTESIAN_POINT('Ctrl Pts',(3.67377298531816,15.5031999223435,-2.59934255826103));
#4637=CARTESIAN_POINT('Ctrl Pts',(4.5183505797536,15.6281999223435,-1.40566135584279));
#4638=CARTESIAN_POINT('Ctrl Pts',(4.5,15.7531999223435,0.0564772772052848));
#4639=CARTESIAN_POINT('Ctrl Pts',(4.4816494202464,15.8781999223435,1.51861591025336));
#4640=CARTESIAN_POINT('Ctrl Pts',(3.60737996405636,16.0031999223435,2.69072471237123));
#4641=CARTESIAN_POINT('Ctrl Pts',(2.73311050786633,16.1281999223435,3.8628335144891));
#4642=CARTESIAN_POINT('Ctrl Pts',(1.33686339217857,16.2531999223435,4.29720676178065));
#4643=CARTESIAN_POINT('Ctrl Pts',(-0.0593837235091896,16.3781999223435,
4.7315800090722));
#4644=CARTESIAN_POINT('Ctrl Pts',(-1.44428955719596,16.5031999223435,4.26230188487573));
#4645=CARTESIAN_POINT('Ctrl Pts',(-2.82919539088272,16.6281999223435,3.79302376067927));
#4646=CARTESIAN_POINT('Ctrl Pts',(-3.67377298531816,16.7531999223435,2.59934255826103));
#4647=CARTESIAN_POINT('Ctrl Pts',(-4.5183505797536,16.8781999223435,1.40566135584279));
#4648=CARTESIAN_POINT('Ctrl Pts',(-4.5,17.0031999223435,-0.0564772772052853));
#4649=CARTESIAN_POINT('Ctrl Pts',(-4.4816494202464,17.1281999223435,-1.51861591025336));
#4650=CARTESIAN_POINT('Ctrl Pts',(-3.60737996405636,17.2531999223435,-2.69072471237123));
#4651=CARTESIAN_POINT('Ctrl Pts',(-2.73311050786633,17.3781999223435,-3.8628335144891));
#4652=CARTESIAN_POINT('Ctrl Pts',(-1.33686339217857,17.5031999223435,-4.29720676178065));
#4653=CARTESIAN_POINT('Ctrl Pts',(0.0593837235091902,17.6281999223435,-4.7315800090722));
#4654=CARTESIAN_POINT('Ctrl Pts',(1.44428955719596,17.7531999223435,-4.26230188487573));
#4655=CARTESIAN_POINT('Ctrl Pts',(2.82919539088272,17.8781999223435,-3.79302376067926));
#4656=CARTESIAN_POINT('Ctrl Pts',(3.67377298531816,18.0031999223435,-2.59934255826103));
#4657=CARTESIAN_POINT('Ctrl Pts',(4.5183505797536,18.1281999223435,-1.40566135584279));
#4658=CARTESIAN_POINT('Ctrl Pts',(4.5,18.2531999223435,0.0564772772052848));
#4659=CARTESIAN_POINT('Ctrl Pts',(4.4816494202464,18.3781999223435,1.51861591025336));
#4660=CARTESIAN_POINT('Ctrl Pts',(3.60737996405636,18.5031999223435,2.69072471237123));
#4661=CARTESIAN_POINT('Ctrl Pts',(2.73311050786633,18.6281999223435,3.8628335144891));
#4662=CARTESIAN_POINT('Ctrl Pts',(1.33686339217857,18.7531999223435,4.29720676178065));
#4663=CARTESIAN_POINT('Ctrl Pts',(-0.0593837235091896,18.8781999223435,
4.7315800090722));
#4664=CARTESIAN_POINT('Ctrl Pts',(-1.44428955719596,19.0031999223435,4.26230188487573));
#4665=CARTESIAN_POINT('Ctrl Pts',(-2.82919539088272,19.1281999223435,3.79302376067927));
#4666=CARTESIAN_POINT('Ctrl Pts',(-3.67377298531816,19.2531999223435,2.59934255826103));
#4667=CARTESIAN_POINT('Ctrl Pts',(-4.5183505797536,19.3781999223435,1.40566135584279));
#4668=CARTESIAN_POINT('Ctrl Pts',(-4.5,19.5031999223435,-0.0564772772052853));
#4669=CARTESIAN_POINT('Ctrl Pts',(-4.4816494202464,19.6281999223435,-1.51861591025336));
#4670=CARTESIAN_POINT('Ctrl Pts',(-3.60737996405636,19.7531999223435,-2.69072471237123));
#4671=CARTESIAN_POINT('Ctrl Pts',(-2.73311050786633,19.8781999223435,-3.8628335144891));
#4672=CARTESIAN_POINT('Ctrl Pts',(-1.33686339217857,20.0031999223435,-4.29720676178065));
#4673=CARTESIAN_POINT('Ctrl Pts',(0.0593837235091902,20.1281999223435,-4.7315800090722));
#4674=CARTESIAN_POINT('Ctrl Pts',(1.44428955719596,20.2531999223435,-4.26230188487573));
#4675=CARTESIAN_POINT('Ctrl Pts',(2.82919539088272,20.3781999223435,-3.79302376067926));
#4676=CARTESIAN_POINT('Ctrl Pts',(3.67377298531816,20.5031999223435,-2.59934255826103));
#4677=CARTESIAN_POINT('Ctrl Pts',(4.5183505797536,20.6281999223435,-1.40566135584279));
#4678=CARTESIAN_POINT('Ctrl Pts',(4.5,20.7531999223435,0.0564772772052848));
#4679=CARTESIAN_POINT('Ctrl Pts',(4.4816494202464,20.8781999223435,1.51861591025336));
#4680=CARTESIAN_POINT('Ctrl Pts',(3.60737996405636,21.0031999223435,2.69072471237123));
#4681=CARTESIAN_POINT('Ctrl Pts',(2.73311050786633,21.1281999223435,3.8628335144891));
#4682=CARTESIAN_POINT('Ctrl Pts',(1.33686339217857,21.2531999223435,4.29720676178065));
#4683=CARTESIAN_POINT('Ctrl Pts',(-0.0593837235091896,21.3781999223435,
4.7315800090722));
#4684=CARTESIAN_POINT('Ctrl Pts',(-1.44428955719596,21.5031999223435,4.26230188487573));
#4685=CARTESIAN_POINT('Ctrl Pts',(-2.82919539088272,21.6281999223435,3.79302376067927));
#4686=CARTESIAN_POINT('Ctrl Pts',(-3.67377298531816,21.7531999223435,2.59934255826103));
#4687=CARTESIAN_POINT('Ctrl Pts',(-4.5183505797536,21.8781999223435,1.40566135584279));
#4688=CARTESIAN_POINT('Ctrl Pts',(-4.5,22.0031999223435,-0.0564772772052853));
#4689=CARTESIAN_POINT('Ctrl Pts',(-4.4816494202464,22.1281999223435,-1.51861591025336));
#4690=CARTESIAN_POINT('Ctrl Pts',(-3.60737996405636,22.2531999223435,-2.69072471237123));
#4691=CARTESIAN_POINT('Ctrl Pts',(-2.73311050786633,22.3781999223435,-3.8628335144891));
#4692=CARTESIAN_POINT('Ctrl Pts',(-1.33686339217857,22.5031999223435,-4.29720676178065));
#4693=CARTESIAN_POINT('Ctrl Pts',(0.0593837235091902,22.6281999223435,-4.7315800090722));
#4694=CARTESIAN_POINT('Ctrl Pts',(1.44428955719596,22.7531999223435,-4.26230188487573));
#4695=CARTESIAN_POINT('Ctrl Pts',(2.82919539088272,22.8781999223435,-3.79302376067926));
#4696=CARTESIAN_POINT('Ctrl Pts',(3.67377298531816,23.0031999223435,-2.59934255826103));
#4697=CARTESIAN_POINT('Ctrl Pts',(4.5183505797536,23.1281999223435,-1.40566135584279));
#4698=CARTESIAN_POINT('Ctrl Pts',(4.5,23.2531999223435,0.0564772772052848));
#4699=CARTESIAN_POINT('Ctrl Pts',(4.4816494202464,23.3781999223435,1.51861591025336));
#4700=CARTESIAN_POINT('Ctrl Pts',(3.60737996405636,23.5031999223435,2.69072471237123));
#4701=CARTESIAN_POINT('Ctrl Pts',(2.73311050786633,23.6281999223435,3.8628335144891));
#4702=CARTESIAN_POINT('Ctrl Pts',(1.33686339217857,23.7531999223435,4.29720676178065));
#4703=CARTESIAN_POINT('Ctrl Pts',(-0.0593837235091896,23.8781999223435,
4.7315800090722));
#4704=CARTESIAN_POINT('Ctrl Pts',(-1.44428955719596,24.0031999223435,4.26230188487573));
#4705=CARTESIAN_POINT('Ctrl Pts',(-2.82919539088272,24.1281999223435,3.79302376067927));
#4706=CARTESIAN_POINT('Ctrl Pts',(-3.67377298531816,24.2531999223435,2.59934255826103));
#4707=CARTESIAN_POINT('Ctrl Pts',(-4.5183505797536,24.3781999223435,1.40566135584279));
#4708=CARTESIAN_POINT('Ctrl Pts',(-4.5,24.5031999223436,-0.0564772772052853));
#4709=CARTESIAN_POINT('Ctrl Pts',(-4.4816494202464,24.6281999223435,-1.51861591025336));
#4710=CARTESIAN_POINT('Ctrl Pts',(-3.60737996405636,24.7531999223435,-2.69072471237123));
#4711=CARTESIAN_POINT('Ctrl Pts',(-2.73311050786633,24.8781999223436,-3.8628335144891));
#4712=CARTESIAN_POINT('Ctrl Pts',(-1.33686339217857,25.0031999223435,-4.29720676178065));
#4713=CARTESIAN_POINT('Ctrl Pts',(0.0593837235091902,25.1281999223435,-4.7315800090722));
#4714=CARTESIAN_POINT('Ctrl Pts',(1.44428955719596,25.2531999223435,-4.26230188487573));
#4715=CARTESIAN_POINT('Ctrl Pts',(2.82919539088272,25.3781999223435,-3.79302376067926));
#4716=CARTESIAN_POINT('Ctrl Pts',(3.67377298531816,25.5031999223435,-2.59934255826103));
#4717=CARTESIAN_POINT('Ctrl Pts',(4.5183505797536,25.6281999223435,-1.40566135584279));
#4718=CARTESIAN_POINT('Ctrl Pts',(4.5,25.7531999223436,0.0564772772052848));
#4719=CARTESIAN_POINT('Ctrl Pts',(4.4816494202464,25.8781999223436,1.51861591025336));
#4720=CARTESIAN_POINT('Ctrl Pts',(3.60737996405636,26.0031999223435,2.69072471237123));
#4721=CARTESIAN_POINT('Ctrl Pts',(2.73311050786633,26.1281999223435,3.8628335144891));
#4722=CARTESIAN_POINT('Ctrl Pts',(1.33686339217857,26.2531999223435,4.29720676178065));
#4723=CARTESIAN_POINT('Ctrl Pts',(-0.0593837235091896,26.3781999223436,
4.7315800090722));
#4724=CARTESIAN_POINT('Ctrl Pts',(-1.44428955719596,26.5031999223435,4.26230188487573));
#4725=CARTESIAN_POINT('Ctrl Pts',(-2.82919539088272,26.6281999223435,3.79302376067927));
#4726=CARTESIAN_POINT('Ctrl Pts',(-3.67377298531816,26.7531999223436,2.59934255826103));
#4727=CARTESIAN_POINT('Ctrl Pts',(-4.5183505797536,26.8781999223435,1.40566135584279));
#4728=CARTESIAN_POINT('Ctrl Pts',(-4.5,27.0031999223436,-0.0564772772052853));
#4729=CARTESIAN_POINT('Ctrl Pts',(-4.4816494202464,27.1281999223436,-1.51861591025336));
#4730=CARTESIAN_POINT('Ctrl Pts',(-3.60737996405636,27.2531999223435,-2.69072471237123));
#4731=CARTESIAN_POINT('Ctrl Pts',(-2.73311050786633,27.3781999223436,-3.8628335144891));
#4732=CARTESIAN_POINT('Ctrl Pts',(-1.33686339217857,27.5031999223435,-4.29720676178065));
#4733=CARTESIAN_POINT('Ctrl Pts',(0.0593837235091902,27.6281999223435,-4.7315800090722));
#4734=CARTESIAN_POINT('Ctrl Pts',(1.44428955719596,27.7531999223435,-4.26230188487573));
#4735=CARTESIAN_POINT('Ctrl Pts',(2.82919539088272,27.8781999223435,-3.79302376067926));
#4736=CARTESIAN_POINT('Ctrl Pts',(3.67377298531816,28.0031999223436,-2.59934255826103));
#4737=CARTESIAN_POINT('Ctrl Pts',(4.5183505797536,28.1281999223435,-1.40566135584279));
#4738=CARTESIAN_POINT('Ctrl Pts',(4.5,28.2531999223435,0.0564772772052848));
#4739=CARTESIAN_POINT('Ctrl Pts',(4.4816494202464,28.3781999223436,1.51861591025336));
#4740=CARTESIAN_POINT('Ctrl Pts',(3.60737996405636,28.5031999223435,2.69072471237123));
#4741=CARTESIAN_POINT('Ctrl Pts',(2.73311050786633,28.6281999223435,3.8628335144891));
#4742=CARTESIAN_POINT('Ctrl Pts',(1.33686339217857,28.7531999223435,4.29720676178065));
#4743=CARTESIAN_POINT('Ctrl Pts',(-0.0593837235091896,28.8781999223435,
4.7315800090722));
#4744=CARTESIAN_POINT('Ctrl Pts',(-1.44428955719596,29.0031999223435,4.26230188487573));
#4745=CARTESIAN_POINT('Ctrl Pts',(-2.82919539088272,29.1281999223435,3.79302376067927));
#4746=CARTESIAN_POINT('Ctrl Pts',(-3.67377298531816,29.2531999223435,2.59934255826103));
#4747=CARTESIAN_POINT('Ctrl Pts',(-4.5183505797536,29.3781999223436,1.40566135584279));
#4748=CARTESIAN_POINT('Ctrl Pts',(-4.5,29.5031999223435,-0.0564772772052853));
#4749=CARTESIAN_POINT('Ctrl Pts',(-4.4816494202464,29.6281999223435,-1.51861591025336));
#4750=CARTESIAN_POINT('Ctrl Pts',(-3.60737996405636,29.7531999223435,-2.69072471237123));
#4751=CARTESIAN_POINT('Ctrl Pts',(-2.73311050786633,29.8781999223435,-3.8628335144891));
#4752=CARTESIAN_POINT('Ctrl Pts',(-1.33686339217857,30.0031999223435,-4.29720676178065));
#4753=CARTESIAN_POINT('Ctrl Pts',(0.0593837235091902,30.1281999223435,-4.7315800090722));
#4754=CARTESIAN_POINT('Ctrl Pts',(1.44428955719596,30.2531999223435,-4.26230188487573));
#4755=CARTESIAN_POINT('Ctrl Pts',(2.82919539088272,30.3781999223435,-3.79302376067926));
#4756=CARTESIAN_POINT('Ctrl Pts',(3.67377298531816,30.5031999223435,-2.59934255826103));
#4757=CARTESIAN_POINT('Ctrl Pts',(4.5183505797536,30.6281999223435,-1.40566135584279));
#4758=CARTESIAN_POINT('Ctrl Pts',(4.5,30.7531999223435,0.0564772772052848));
#4759=CARTESIAN_POINT('Ctrl Pts',(4.4816494202464,30.8781999223435,1.51861591025336));
#4760=CARTESIAN_POINT('Ctrl Pts',(3.60737996405636,31.0031999223435,2.69072471237123));
#4761=CARTESIAN_POINT('Ctrl Pts',(2.73311050786633,31.1281999223435,3.8628335144891));
#4762=CARTESIAN_POINT('Ctrl Pts',(1.33686339217857,31.2531999223435,4.29720676178065));
#4763=CARTESIAN_POINT('Ctrl Pts',(-0.0593837235091896,31.3781999223435,
4.7315800090722));
#4764=CARTESIAN_POINT('Ctrl Pts',(-1.44428955719596,31.5031999223435,4.26230188487573));
#4765=CARTESIAN_POINT('Ctrl Pts',(-2.82919539088272,31.6281999223435,3.79302376067927));
#4766=CARTESIAN_POINT('Ctrl Pts',(-3.67377298531816,31.7531999223436,2.59934255826103));
#4767=CARTESIAN_POINT('Ctrl Pts',(-4.5183505797536,31.8781999223435,1.40566135584279));
#4768=CARTESIAN_POINT('Ctrl Pts',(-4.5,32.0031999223435,-0.0564772772052853));
#4769=CARTESIAN_POINT('Ctrl Pts',(-4.4816494202464,32.1281999223435,-1.51861591025336));
#4770=CARTESIAN_POINT('Ctrl Pts',(-3.60737996405636,32.2531999223435,-2.69072471237123));
#4771=CARTESIAN_POINT('Ctrl Pts',(-2.73311050786633,32.3781999223435,-3.8628335144891));
#4772=CARTESIAN_POINT('Ctrl Pts',(-1.33686339217857,32.5031999223435,-4.29720676178065));
#4773=CARTESIAN_POINT('Ctrl Pts',(0.0593837235091902,32.6281999223435,-4.7315800090722));
#4774=CARTESIAN_POINT('Ctrl Pts',(1.44428955719596,32.7531999223435,-4.26230188487573));
#4775=CARTESIAN_POINT('Ctrl Pts',(2.82919539088272,32.8781999223435,-3.79302376067926));
#4776=CARTESIAN_POINT('Ctrl Pts',(3.67377298531816,33.0031999223436,-2.59934255826103));
#4777=CARTESIAN_POINT('Ctrl Pts',(4.5183505797536,33.1281999223435,-1.40566135584279));
#4778=CARTESIAN_POINT('Ctrl Pts',(4.5,33.2531999223435,0.0564772772052848));
#4779=CARTESIAN_POINT('Ctrl Pts',(4.4816494202464,33.3781999223435,1.51861591025336));
#4780=CARTESIAN_POINT('Ctrl Pts',(3.60737996405636,33.5031999223435,2.69072471237123));
#4781=CARTESIAN_POINT('Ctrl Pts',(2.73311050786633,33.6281999223436,3.8628335144891));
#4782=CARTESIAN_POINT('Ctrl Pts',(1.33686339217857,33.7531999223435,4.29720676178065));
#4783=CARTESIAN_POINT('Ctrl Pts',(-0.0593837235091896,33.8781999223435,
4.7315800090722));
#4784=CARTESIAN_POINT('Ctrl Pts',(-1.44428955719596,34.0031999223435,4.26230188487573));
#4785=CARTESIAN_POINT('Ctrl Pts',(-2.82919539088272,34.1281999223435,3.79302376067927));
#4786=CARTESIAN_POINT('Ctrl Pts',(-3.67377298531816,34.2531999223435,2.59934255826103));
#4787=CARTESIAN_POINT('Ctrl Pts',(-4.5183505797536,34.3781999223435,1.40566135584279));
#4788=CARTESIAN_POINT('Ctrl Pts',(-4.5,34.5031999223435,-0.0564772772052853));
#4789=CARTESIAN_POINT('Ctrl Pts',(-4.4816494202464,34.6281999223435,-1.51861591025336));
#4790=CARTESIAN_POINT('Ctrl Pts',(-3.60737996405636,34.7531999223435,-2.69072471237123));
#4791=CARTESIAN_POINT('Ctrl Pts',(-2.73311050786633,34.8781999223436,-3.8628335144891));
#4792=CARTESIAN_POINT('Ctrl Pts',(-1.33686339217857,35.0031999223435,-4.29720676178065));
#4793=CARTESIAN_POINT('Ctrl Pts',(0.0593837235091902,35.1281999223435,-4.7315800090722));
#4794=CARTESIAN_POINT('Ctrl Pts',(1.44428955719596,35.2531999223435,-4.26230188487573));
#4795=CARTESIAN_POINT('Ctrl Pts',(2.82919539088272,35.3781999223435,-3.79302376067926));
#4796=CARTESIAN_POINT('Ctrl Pts',(3.67377298531816,35.5031999223436,-2.59934255826103));
#4797=CARTESIAN_POINT('Ctrl Pts',(4.5183505797536,35.6281999223435,-1.40566135584279));
#4798=CARTESIAN_POINT('Ctrl Pts',(4.5,35.7531999223435,0.0564772772052848));
#4799=CARTESIAN_POINT('Ctrl Pts',(4.4816494202464,35.8781999223435,1.51861591025336));
#4800=CARTESIAN_POINT('Ctrl Pts',(3.60737996405636,36.0031999223435,2.69072471237123));
#4801=CARTESIAN_POINT('Ctrl Pts',(2.73311050786633,36.1281999223436,3.8628335144891));
#4802=CARTESIAN_POINT('Ctrl Pts',(1.33686339217857,36.2531999223435,4.29720676178065));
#4803=CARTESIAN_POINT('Ctrl Pts',(-0.0593837235091896,36.3781999223435,
4.7315800090722));
#4804=CARTESIAN_POINT('Ctrl Pts',(-1.44428955719596,36.5031999223435,4.26230188487573));
#4805=CARTESIAN_POINT('Ctrl Pts',(-2.82919539088272,36.6281999223435,3.79302376067927));
#4806=CARTESIAN_POINT('Ctrl Pts',(-3.67377298531816,36.7531999223435,2.59934255826103));
#4807=CARTESIAN_POINT('Ctrl Pts',(-4.5183505797536,36.8781999223435,1.40566135584279));
#4808=CARTESIAN_POINT('Ctrl Pts',(-4.5,37.0031999223435,-0.0564772772052853));
#4809=CARTESIAN_POINT('Ctrl Pts',(-4.4816494202464,37.1281999223435,-1.51861591025336));
#4810=CARTESIAN_POINT('Ctrl Pts',(-3.60737996405636,37.2531999223435,-2.69072471237123));
#4811=CARTESIAN_POINT('Ctrl Pts',(-2.73311050786633,37.3781999223436,-3.8628335144891));
#4812=CARTESIAN_POINT('Ctrl Pts',(-1.33686339217857,37.5031999223435,-4.29720676178065));
#4813=CARTESIAN_POINT('Ctrl Pts',(0.0593837235091902,37.6281999223435,-4.7315800090722));
#4814=CARTESIAN_POINT('Ctrl Pts',(1.44428955719596,37.7531999223435,-4.26230188487573));
#4815=CARTESIAN_POINT('Ctrl Pts',(2.82919539088272,37.8781999223435,-3.79302376067926));
#4816=CARTESIAN_POINT('Ctrl Pts',(3.67377298531816,38.0031999223435,-2.59934255826103));
#4817=CARTESIAN_POINT('Ctrl Pts',(4.5183505797536,38.1281999223435,-1.40566135584279));
#4818=CARTESIAN_POINT('Ctrl Pts',(4.5,38.2531999223435,0.0564772772052848));
#4819=CARTESIAN_POINT('Ctrl Pts',(4.4816494202464,38.3781999223435,1.51861591025336));
#4820=CARTESIAN_POINT('Ctrl Pts',(3.60737996405636,38.5031999223435,2.69072471237123));
#4821=CARTESIAN_POINT('Ctrl Pts',(2.73311050786633,38.6281999223436,3.8628335144891));
#4822=CARTESIAN_POINT('Ctrl Pts',(1.33686339217857,38.7531999223435,4.29720676178065));
#4823=CARTESIAN_POINT('Ctrl Pts',(-0.0593837235091896,38.8781999223435,
4.7315800090722));
#4824=CARTESIAN_POINT('Ctrl Pts',(-1.44428955719596,39.0031999223435,4.26230188487573));
#4825=CARTESIAN_POINT('Ctrl Pts',(-2.82919539088272,39.1281999223435,3.79302376067927));
#4826=CARTESIAN_POINT('Ctrl Pts',(-3.67377298531816,39.2531999223436,2.59934255826103));
#4827=CARTESIAN_POINT('Ctrl Pts',(-4.5183505797536,39.3781999223435,1.40566135584279));
#4828=CARTESIAN_POINT('Ctrl Pts',(-4.5,39.5031999223435,-0.0564772772052853));
#4829=CARTESIAN_POINT('Ctrl Pts',(-4.5,15.4968000776565,0.0564772772053793));
#4830=CARTESIAN_POINT('Ctrl Pts',(-4.51835057975363,15.6218000776565,-1.4056613558427));
#4831=CARTESIAN_POINT('Ctrl Pts',(-3.67377298531822,15.7468000776565,-2.59934255826095));
#4832=CARTESIAN_POINT('Ctrl Pts',(-2.82919539088281,15.8718000776565,-3.79302376067921));
#4833=CARTESIAN_POINT('Ctrl Pts',(-1.44428955719605,15.9968000776565,-4.2623018848757));
#4834=CARTESIAN_POINT('Ctrl Pts',(-0.0593837235092896,16.1218000776565,
-4.7315800090722));
#4835=CARTESIAN_POINT('Ctrl Pts',(1.33686339217848,16.2468000776565,-4.29720676178068));
#4836=CARTESIAN_POINT('Ctrl Pts',(2.73311050786625,16.3718000776565,-3.86283351448915));
#4837=CARTESIAN_POINT('Ctrl Pts',(3.60737996405631,16.4968000776565,-2.69072471237131));
#4838=CARTESIAN_POINT('Ctrl Pts',(4.48164942024637,16.6218000776565,-1.51861591025346));
#4839=CARTESIAN_POINT('Ctrl Pts',(4.5,16.7468000776565,-0.0564772772053798));
#4840=CARTESIAN_POINT('Ctrl Pts',(4.51835057975363,16.8718000776565,1.4056613558427));
#4841=CARTESIAN_POINT('Ctrl Pts',(3.67377298531822,16.9968000776565,2.59934255826095));
#4842=CARTESIAN_POINT('Ctrl Pts',(2.82919539088281,17.1218000776565,3.7930237606792));
#4843=CARTESIAN_POINT('Ctrl Pts',(1.44428955719605,17.2468000776565,4.2623018848757));
#4844=CARTESIAN_POINT('Ctrl Pts',(0.0593837235092902,17.3718000776565,4.7315800090722));
#4845=CARTESIAN_POINT('Ctrl Pts',(-1.33686339217848,17.4968000776565,4.29720676178068));
#4846=CARTESIAN_POINT('Ctrl Pts',(-2.73311050786625,17.6218000776565,3.86283351448915));
#4847=CARTESIAN_POINT('Ctrl Pts',(-3.60737996405631,17.7468000776565,2.69072471237131));
#4848=CARTESIAN_POINT('Ctrl Pts',(-4.48164942024637,17.8718000776565,1.51861591025346));
#4849=CARTESIAN_POINT('Ctrl Pts',(-4.5,17.9968000776565,0.0564772772053793));
#4850=CARTESIAN_POINT('Ctrl Pts',(-4.51835057975363,18.1218000776565,-1.4056613558427));
#4851=CARTESIAN_POINT('Ctrl Pts',(-3.67377298531822,18.2468000776565,-2.59934255826095));
#4852=CARTESIAN_POINT('Ctrl Pts',(-2.82919539088281,18.3718000776565,-3.79302376067921));
#4853=CARTESIAN_POINT('Ctrl Pts',(-1.44428955719605,18.4968000776565,-4.2623018848757));
#4854=CARTESIAN_POINT('Ctrl Pts',(-0.0593837235092896,18.6218000776565,
-4.7315800090722));
#4855=CARTESIAN_POINT('Ctrl Pts',(1.33686339217848,18.7468000776565,-4.29720676178068));
#4856=CARTESIAN_POINT('Ctrl Pts',(2.73311050786625,18.8718000776565,-3.86283351448915));
#4857=CARTESIAN_POINT('Ctrl Pts',(3.60737996405631,18.9968000776565,-2.69072471237131));
#4858=CARTESIAN_POINT('Ctrl Pts',(4.48164942024637,19.1218000776565,-1.51861591025346));
#4859=CARTESIAN_POINT('Ctrl Pts',(4.5,19.2468000776565,-0.0564772772053798));
#4860=CARTESIAN_POINT('Ctrl Pts',(4.51835057975363,19.3718000776565,1.4056613558427));
#4861=CARTESIAN_POINT('Ctrl Pts',(3.67377298531822,19.4968000776565,2.59934255826095));
#4862=CARTESIAN_POINT('Ctrl Pts',(2.82919539088281,19.6218000776565,3.7930237606792));
#4863=CARTESIAN_POINT('Ctrl Pts',(1.44428955719605,19.7468000776565,4.2623018848757));
#4864=CARTESIAN_POINT('Ctrl Pts',(0.0593837235092902,19.8718000776565,4.7315800090722));
#4865=CARTESIAN_POINT('Ctrl Pts',(-1.33686339217848,19.9968000776565,4.29720676178068));
#4866=CARTESIAN_POINT('Ctrl Pts',(-2.73311050786625,20.1218000776565,3.86283351448915));
#4867=CARTESIAN_POINT('Ctrl Pts',(-3.60737996405631,20.2468000776565,2.69072471237131));
#4868=CARTESIAN_POINT('Ctrl Pts',(-4.48164942024637,20.3718000776565,1.51861591025346));
#4869=CARTESIAN_POINT('Ctrl Pts',(-4.5,20.4968000776565,0.0564772772053793));
#4870=CARTESIAN_POINT('Ctrl Pts',(-4.51835057975363,20.6218000776565,-1.4056613558427));
#4871=CARTESIAN_POINT('Ctrl Pts',(-3.67377298531822,20.7468000776565,-2.59934255826095));
#4872=CARTESIAN_POINT('Ctrl Pts',(-2.82919539088281,20.8718000776565,-3.79302376067921));
#4873=CARTESIAN_POINT('Ctrl Pts',(-1.44428955719605,20.9968000776565,-4.2623018848757));
#4874=CARTESIAN_POINT('Ctrl Pts',(-0.0593837235092896,21.1218000776565,
-4.7315800090722));
#4875=CARTESIAN_POINT('Ctrl Pts',(1.33686339217848,21.2468000776565,-4.29720676178068));
#4876=CARTESIAN_POINT('Ctrl Pts',(2.73311050786625,21.3718000776565,-3.86283351448915));
#4877=CARTESIAN_POINT('Ctrl Pts',(3.60737996405631,21.4968000776565,-2.69072471237131));
#4878=CARTESIAN_POINT('Ctrl Pts',(4.48164942024637,21.6218000776565,-1.51861591025346));
#4879=CARTESIAN_POINT('Ctrl Pts',(4.5,21.7468000776565,-0.0564772772053798));
#4880=CARTESIAN_POINT('Ctrl Pts',(4.51835057975363,21.8718000776565,1.4056613558427));
#4881=CARTESIAN_POINT('Ctrl Pts',(3.67377298531822,21.9968000776565,2.59934255826095));
#4882=CARTESIAN_POINT('Ctrl Pts',(2.82919539088281,22.1218000776565,3.7930237606792));
#4883=CARTESIAN_POINT('Ctrl Pts',(1.44428955719605,22.2468000776565,4.2623018848757));
#4884=CARTESIAN_POINT('Ctrl Pts',(0.0593837235092902,22.3718000776565,4.7315800090722));
#4885=CARTESIAN_POINT('Ctrl Pts',(-1.33686339217848,22.4968000776565,4.29720676178068));
#4886=CARTESIAN_POINT('Ctrl Pts',(-2.73311050786625,22.6218000776565,3.86283351448915));
#4887=CARTESIAN_POINT('Ctrl Pts',(-3.60737996405631,22.7468000776565,2.69072471237131));
#4888=CARTESIAN_POINT('Ctrl Pts',(-4.48164942024637,22.8718000776565,1.51861591025346));
#4889=CARTESIAN_POINT('Ctrl Pts',(-4.5,22.9968000776565,0.0564772772053793));
#4890=CARTESIAN_POINT('Ctrl Pts',(-4.51835057975363,23.1218000776565,-1.4056613558427));
#4891=CARTESIAN_POINT('Ctrl Pts',(-3.67377298531822,23.2468000776565,-2.59934255826095));
#4892=CARTESIAN_POINT('Ctrl Pts',(-2.82919539088281,23.3718000776565,-3.79302376067921));
#4893=CARTESIAN_POINT('Ctrl Pts',(-1.44428955719605,23.4968000776565,-4.2623018848757));
#4894=CARTESIAN_POINT('Ctrl Pts',(-0.0593837235092896,23.6218000776565,
-4.7315800090722));
#4895=CARTESIAN_POINT('Ctrl Pts',(1.33686339217848,23.7468000776565,-4.29720676178068));
#4896=CARTESIAN_POINT('Ctrl Pts',(2.73311050786625,23.8718000776565,-3.86283351448915));
#4897=CARTESIAN_POINT('Ctrl Pts',(3.60737996405631,23.9968000776565,-2.69072471237131));
#4898=CARTESIAN_POINT('Ctrl Pts',(4.48164942024637,24.1218000776565,-1.51861591025346));
#4899=CARTESIAN_POINT('Ctrl Pts',(4.5,24.2468000776565,-0.0564772772053798));
#4900=CARTESIAN_POINT('Ctrl Pts',(4.51835057975363,24.3718000776565,1.4056613558427));
#4901=CARTESIAN_POINT('Ctrl Pts',(3.67377298531822,24.4968000776565,2.59934255826095));
#4902=CARTESIAN_POINT('Ctrl Pts',(2.82919539088281,24.6218000776565,3.7930237606792));
#4903=CARTESIAN_POINT('Ctrl Pts',(1.44428955719605,24.7468000776565,4.2623018848757));
#4904=CARTESIAN_POINT('Ctrl Pts',(0.0593837235092902,24.8718000776565,4.7315800090722));
#4905=CARTESIAN_POINT('Ctrl Pts',(-1.33686339217848,24.9968000776565,4.29720676178068));
#4906=CARTESIAN_POINT('Ctrl Pts',(-2.73311050786625,25.1218000776565,3.86283351448915));
#4907=CARTESIAN_POINT('Ctrl Pts',(-3.60737996405631,25.2468000776565,2.69072471237131));
#4908=CARTESIAN_POINT('Ctrl Pts',(-4.48164942024637,25.3718000776565,1.51861591025346));
#4909=CARTESIAN_POINT('Ctrl Pts',(-4.5,25.4968000776565,0.0564772772053793));
#4910=CARTESIAN_POINT('Ctrl Pts',(-4.51835057975363,25.6218000776565,-1.4056613558427));
#4911=CARTESIAN_POINT('Ctrl Pts',(-3.67377298531822,25.7468000776565,-2.59934255826095));
#4912=CARTESIAN_POINT('Ctrl Pts',(-2.82919539088281,25.8718000776565,-3.79302376067921));
#4913=CARTESIAN_POINT('Ctrl Pts',(-1.44428955719605,25.9968000776565,-4.2623018848757));
#4914=CARTESIAN_POINT('Ctrl Pts',(-0.0593837235092896,26.1218000776565,
-4.7315800090722));
#4915=CARTESIAN_POINT('Ctrl Pts',(1.33686339217848,26.2468000776565,-4.29720676178068));
#4916=CARTESIAN_POINT('Ctrl Pts',(2.73311050786625,26.3718000776565,-3.86283351448915));
#4917=CARTESIAN_POINT('Ctrl Pts',(3.60737996405631,26.4968000776565,-2.69072471237131));
#4918=CARTESIAN_POINT('Ctrl Pts',(4.48164942024637,26.6218000776565,-1.51861591025346));
#4919=CARTESIAN_POINT('Ctrl Pts',(4.5,26.7468000776565,-0.0564772772053798));
#4920=CARTESIAN_POINT('Ctrl Pts',(4.51835057975363,26.8718000776565,1.4056613558427));
#4921=CARTESIAN_POINT('Ctrl Pts',(3.67377298531822,26.9968000776565,2.59934255826095));
#4922=CARTESIAN_POINT('Ctrl Pts',(2.82919539088281,27.1218000776565,3.7930237606792));
#4923=CARTESIAN_POINT('Ctrl Pts',(1.44428955719605,27.2468000776565,4.2623018848757));
#4924=CARTESIAN_POINT('Ctrl Pts',(0.0593837235092902,27.3718000776565,4.7315800090722));
#4925=CARTESIAN_POINT('Ctrl Pts',(-1.33686339217848,27.4968000776565,4.29720676178068));
#4926=CARTESIAN_POINT('Ctrl Pts',(-2.73311050786625,27.6218000776565,3.86283351448915));
#4927=CARTESIAN_POINT('Ctrl Pts',(-3.60737996405631,27.7468000776565,2.69072471237131));
#4928=CARTESIAN_POINT('Ctrl Pts',(-4.48164942024637,27.8718000776565,1.51861591025346));
#4929=CARTESIAN_POINT('Ctrl Pts',(-4.5,27.9968000776565,0.0564772772053793));
#4930=CARTESIAN_POINT('Ctrl Pts',(-4.51835057975363,28.1218000776565,-1.4056613558427));
#4931=CARTESIAN_POINT('Ctrl Pts',(-3.67377298531822,28.2468000776565,-2.59934255826095));
#4932=CARTESIAN_POINT('Ctrl Pts',(-2.82919539088281,28.3718000776565,-3.79302376067921));
#4933=CARTESIAN_POINT('Ctrl Pts',(-1.44428955719605,28.4968000776565,-4.2623018848757));
#4934=CARTESIAN_POINT('Ctrl Pts',(-0.0593837235092896,28.6218000776565,
-4.7315800090722));
#4935=CARTESIAN_POINT('Ctrl Pts',(1.33686339217848,28.7468000776565,-4.29720676178068));
#4936=CARTESIAN_POINT('Ctrl Pts',(2.73311050786625,28.8718000776565,-3.86283351448915));
#4937=CARTESIAN_POINT('Ctrl Pts',(3.60737996405631,28.9968000776565,-2.69072471237131));
#4938=CARTESIAN_POINT('Ctrl Pts',(4.48164942024637,29.1218000776565,-1.51861591025346));
#4939=CARTESIAN_POINT('Ctrl Pts',(4.5,29.2468000776565,-0.0564772772053798));
#4940=CARTESIAN_POINT('Ctrl Pts',(4.51835057975363,29.3718000776565,1.4056613558427));
#4941=CARTESIAN_POINT('Ctrl Pts',(3.67377298531822,29.4968000776565,2.59934255826095));
#4942=CARTESIAN_POINT('Ctrl Pts',(2.82919539088281,29.6218000776565,3.7930237606792));
#4943=CARTESIAN_POINT('Ctrl Pts',(1.44428955719605,29.7468000776565,4.2623018848757));
#4944=CARTESIAN_POINT('Ctrl Pts',(0.0593837235092902,29.8718000776565,4.7315800090722));
#4945=CARTESIAN_POINT('Ctrl Pts',(-1.33686339217848,29.9968000776565,4.29720676178068));
#4946=CARTESIAN_POINT('Ctrl Pts',(-2.73311050786625,30.1218000776565,3.86283351448915));
#4947=CARTESIAN_POINT('Ctrl Pts',(-3.60737996405631,30.2468000776565,2.69072471237131));
#4948=CARTESIAN_POINT('Ctrl Pts',(-4.48164942024637,30.3718000776565,1.51861591025346));
#4949=CARTESIAN_POINT('Ctrl Pts',(-4.5,30.4968000776565,0.0564772772053793));
#4950=CARTESIAN_POINT('Ctrl Pts',(-4.51835057975363,30.6218000776565,-1.4056613558427));
#4951=CARTESIAN_POINT('Ctrl Pts',(-3.67377298531822,30.7468000776565,-2.59934255826095));
#4952=CARTESIAN_POINT('Ctrl Pts',(-2.82919539088281,30.8718000776565,-3.79302376067921));
#4953=CARTESIAN_POINT('Ctrl Pts',(-1.44428955719605,30.9968000776565,-4.2623018848757));
#4954=CARTESIAN_POINT('Ctrl Pts',(-0.0593837235092896,31.1218000776565,
-4.7315800090722));
#4955=CARTESIAN_POINT('Ctrl Pts',(1.33686339217848,31.2468000776565,-4.29720676178068));
#4956=CARTESIAN_POINT('Ctrl Pts',(2.73311050786625,31.3718000776565,-3.86283351448915));
#4957=CARTESIAN_POINT('Ctrl Pts',(3.60737996405631,31.4968000776565,-2.69072471237131));
#4958=CARTESIAN_POINT('Ctrl Pts',(4.48164942024637,31.6218000776565,-1.51861591025346));
#4959=CARTESIAN_POINT('Ctrl Pts',(4.5,31.7468000776565,-0.0564772772053798));
#4960=CARTESIAN_POINT('Ctrl Pts',(4.51835057975363,31.8718000776565,1.4056613558427));
#4961=CARTESIAN_POINT('Ctrl Pts',(3.67377298531822,31.9968000776565,2.59934255826095));
#4962=CARTESIAN_POINT('Ctrl Pts',(2.82919539088281,32.1218000776565,3.7930237606792));
#4963=CARTESIAN_POINT('Ctrl Pts',(1.44428955719605,32.2468000776565,4.2623018848757));
#4964=CARTESIAN_POINT('Ctrl Pts',(0.0593837235092902,32.3718000776565,4.7315800090722));
#4965=CARTESIAN_POINT('Ctrl Pts',(-1.33686339217848,32.4968000776565,4.29720676178068));
#4966=CARTESIAN_POINT('Ctrl Pts',(-2.73311050786625,32.6218000776565,3.86283351448915));
#4967=CARTESIAN_POINT('Ctrl Pts',(-3.60737996405631,32.7468000776565,2.69072471237131));
#4968=CARTESIAN_POINT('Ctrl Pts',(-4.48164942024637,32.8718000776565,1.51861591025346));
#4969=CARTESIAN_POINT('Ctrl Pts',(-4.5,32.9968000776565,0.0564772772053793));
#4970=CARTESIAN_POINT('Ctrl Pts',(-4.51835057975363,33.1218000776565,-1.4056613558427));
#4971=CARTESIAN_POINT('Ctrl Pts',(-3.67377298531822,33.2468000776565,-2.59934255826095));
#4972=CARTESIAN_POINT('Ctrl Pts',(-2.82919539088281,33.3718000776565,-3.79302376067921));
#4973=CARTESIAN_POINT('Ctrl Pts',(-1.44428955719605,33.4968000776565,-4.2623018848757));
#4974=CARTESIAN_POINT('Ctrl Pts',(-0.0593837235092896,33.6218000776565,
-4.7315800090722));
#4975=CARTESIAN_POINT('Ctrl Pts',(1.33686339217848,33.7468000776565,-4.29720676178068));
#4976=CARTESIAN_POINT('Ctrl Pts',(2.73311050786625,33.8718000776565,-3.86283351448915));
#4977=CARTESIAN_POINT('Ctrl Pts',(3.60737996405631,33.9968000776565,-2.69072471237131));
#4978=CARTESIAN_POINT('Ctrl Pts',(4.48164942024637,34.1218000776565,-1.51861591025346));
#4979=CARTESIAN_POINT('Ctrl Pts',(4.5,34.2468000776565,-0.0564772772053798));
#4980=CARTESIAN_POINT('Ctrl Pts',(4.51835057975363,34.3718000776565,1.4056613558427));
#4981=CARTESIAN_POINT('Ctrl Pts',(3.67377298531822,34.4968000776565,2.59934255826095));
#4982=CARTESIAN_POINT('Ctrl Pts',(2.82919539088281,34.6218000776565,3.7930237606792));
#4983=CARTESIAN_POINT('Ctrl Pts',(1.44428955719605,34.7468000776565,4.2623018848757));
#4984=CARTESIAN_POINT('Ctrl Pts',(0.0593837235092902,34.8718000776565,4.7315800090722));
#4985=CARTESIAN_POINT('Ctrl Pts',(-1.33686339217848,34.9968000776565,4.29720676178068));
#4986=CARTESIAN_POINT('Ctrl Pts',(-2.73311050786625,35.1218000776565,3.86283351448915));
#4987=CARTESIAN_POINT('Ctrl Pts',(-3.60737996405631,35.2468000776565,2.69072471237131));
#4988=CARTESIAN_POINT('Ctrl Pts',(-4.48164942024637,35.3718000776565,1.51861591025346));
#4989=CARTESIAN_POINT('Ctrl Pts',(-4.5,35.4968000776565,0.0564772772053793));
#4990=CARTESIAN_POINT('Ctrl Pts',(-4.51835057975363,35.6218000776565,-1.4056613558427));
#4991=CARTESIAN_POINT('Ctrl Pts',(-3.67377298531822,35.7468000776565,-2.59934255826095));
#4992=CARTESIAN_POINT('Ctrl Pts',(-2.82919539088281,35.8718000776565,-3.79302376067921));
#4993=CARTESIAN_POINT('Ctrl Pts',(-1.44428955719605,35.9968000776565,-4.2623018848757));
#4994=CARTESIAN_POINT('Ctrl Pts',(-0.0593837235092896,36.1218000776565,
-4.7315800090722));
#4995=CARTESIAN_POINT('Ctrl Pts',(1.33686339217848,36.2468000776565,-4.29720676178068));
#4996=CARTESIAN_POINT('Ctrl Pts',(2.73311050786625,36.3718000776565,-3.86283351448915));
#4997=CARTESIAN_POINT('Ctrl Pts',(3.60737996405631,36.4968000776565,-2.69072471237131));
#4998=CARTESIAN_POINT('Ctrl Pts',(4.48164942024637,36.6218000776565,-1.51861591025346));
#4999=CARTESIAN_POINT('Ctrl Pts',(4.5,36.7468000776565,-0.0564772772053798));
#5000=CARTESIAN_POINT('Ctrl Pts',(4.51835057975363,36.8718000776565,1.4056613558427));
#5001=CARTESIAN_POINT('Ctrl Pts',(3.67377298531822,36.9968000776565,2.59934255826095));
#5002=CARTESIAN_POINT('Ctrl Pts',(2.82919539088281,37.1218000776565,3.7930237606792));
#5003=CARTESIAN_POINT('Ctrl Pts',(1.44428955719605,37.2468000776565,4.2623018848757));
#5004=CARTESIAN_POINT('Ctrl Pts',(0.0593837235092902,37.3718000776565,4.7315800090722));
#5005=CARTESIAN_POINT('Ctrl Pts',(-1.33686339217848,37.4968000776565,4.29720676178068));
#5006=CARTESIAN_POINT('Ctrl Pts',(-2.73311050786625,37.6218000776565,3.86283351448915));
#5007=CARTESIAN_POINT('Ctrl Pts',(-3.60737996405631,37.7468000776565,2.69072471237131));
#5008=CARTESIAN_POINT('Ctrl Pts',(-4.48164942024637,37.8718000776565,1.51861591025346));
#5009=CARTESIAN_POINT('Ctrl Pts',(-4.5,37.9968000776565,0.0564772772053793));
#5010=CARTESIAN_POINT('Ctrl Pts',(-4.51835057975363,38.1218000776565,-1.4056613558427));
#5011=CARTESIAN_POINT('Ctrl Pts',(-3.67377298531822,38.2468000776565,-2.59934255826095));
#5012=CARTESIAN_POINT('Ctrl Pts',(-2.82919539088281,38.3718000776565,-3.79302376067921));
#5013=CARTESIAN_POINT('Ctrl Pts',(-1.44428955719605,38.4968000776565,-4.2623018848757));
#5014=CARTESIAN_POINT('Ctrl Pts',(-0.0593837235092896,38.6218000776565,
-4.7315800090722));
#5015=CARTESIAN_POINT('Ctrl Pts',(1.33686339217848,38.7468000776565,-4.29720676178068));
#5016=CARTESIAN_POINT('Ctrl Pts',(2.73311050786625,38.8718000776565,-3.86283351448915));
#5017=CARTESIAN_POINT('Ctrl Pts',(3.60737996405631,38.9968000776565,-2.69072471237131));
#5018=CARTESIAN_POINT('Ctrl Pts',(4.48164942024637,39.1218000776565,-1.51861591025346));
#5019=CARTESIAN_POINT('Ctrl Pts',(4.5,39.2468000776565,-0.0564772772053798));
#5020=CARTESIAN_POINT('Ctrl Pts',(4.51835057975363,39.3718000776565,1.4056613558427));
#5021=CARTESIAN_POINT('Ctrl Pts',(3.67377298531822,39.4968000776565,2.59934255826095));
#5022=CARTESIAN_POINT('Ctrl Pts',(2.82919539088281,39.6218000776565,3.7930237606792));
#5023=CARTESIAN_POINT('Ctrl Pts',(1.44428955719605,39.7468000776565,4.2623018848757));
#5024=CARTESIAN_POINT('Ctrl Pts',(0.0593837235092902,39.8718000776565,4.7315800090722));
#5025=CARTESIAN_POINT('Ctrl Pts',(-1.33686339217848,39.9968000776565,4.29720676178068));
#5026=CARTESIAN_POINT('Ctrl Pts',(-2.73311050786625,40.1218000776565,3.86283351448915));
#5027=CARTESIAN_POINT('Ctrl Pts',(-3.60737996405631,40.2468000776565,2.69072471237131));
#5028=CARTESIAN_POINT('Ctrl Pts',(-4.48164942024637,40.3718000776565,1.51861591025346));
#5029=CARTESIAN_POINT('Ctrl Pts',(-4.5,40.4968000776565,0.0564772772053793));
#5030=CARTESIAN_POINT('Ctrl Pts',(-3.5,15.4968000776565,0.0564772772053689));
#5031=CARTESIAN_POINT('Ctrl Pts',(-3.51835057975363,15.6218000776565,-1.0807416596098));
#5032=CARTESIAN_POINT('Ctrl Pts',(-2.86475599094327,15.7468000776565,-2.01155730596849));
#5033=CARTESIAN_POINT('Ctrl Pts',(-2.2111614021329,15.8718000776565,-2.94237295232717));
#5034=CARTESIAN_POINT('Ctrl Pts',(-1.13527256282109,15.9968000776565,-3.31124536858055));
#5035=CARTESIAN_POINT('Ctrl Pts',(-0.0593837235092786,16.1218000776565,
-3.68011778483394));
#5036=CARTESIAN_POINT('Ctrl Pts',(1.02784639780354,16.2468000776565,-3.34615024548552));
#5037=CARTESIAN_POINT('Ctrl Pts',(2.11507651911636,16.3718000776565,-3.01218270613711));
#5038=CARTESIAN_POINT('Ctrl Pts',(2.79836296968137,16.4968000776565,-2.10293946007882));
#5039=CARTESIAN_POINT('Ctrl Pts',(3.48164942024637,16.6218000776565,-1.19369621402054));
#5040=CARTESIAN_POINT('Ctrl Pts',(3.5,16.7468000776565,-0.0564772772053694));
#5041=CARTESIAN_POINT('Ctrl Pts',(3.51835057975363,16.8718000776565,1.0807416596098));
#5042=CARTESIAN_POINT('Ctrl Pts',(2.86475599094327,16.9968000776565,2.01155730596849));
#5043=CARTESIAN_POINT('Ctrl Pts',(2.2111614021329,17.1218000776565,2.94237295232717));
#5044=CARTESIAN_POINT('Ctrl Pts',(1.13527256282109,17.2468000776565,3.31124536858055));
#5045=CARTESIAN_POINT('Ctrl Pts',(0.0593837235092791,17.3718000776565,3.68011778483394));
#5046=CARTESIAN_POINT('Ctrl Pts',(-1.02784639780354,17.4968000776565,3.34615024548552));
#5047=CARTESIAN_POINT('Ctrl Pts',(-2.11507651911636,17.6218000776565,3.01218270613711));
#5048=CARTESIAN_POINT('Ctrl Pts',(-2.79836296968137,17.7468000776565,2.10293946007882));
#5049=CARTESIAN_POINT('Ctrl Pts',(-3.48164942024637,17.8718000776565,1.19369621402054));
#5050=CARTESIAN_POINT('Ctrl Pts',(-3.5,17.9968000776565,0.0564772772053689));
#5051=CARTESIAN_POINT('Ctrl Pts',(-3.51835057975363,18.1218000776565,-1.0807416596098));
#5052=CARTESIAN_POINT('Ctrl Pts',(-2.86475599094327,18.2468000776565,-2.01155730596849));
#5053=CARTESIAN_POINT('Ctrl Pts',(-2.2111614021329,18.3718000776565,-2.94237295232717));
#5054=CARTESIAN_POINT('Ctrl Pts',(-1.13527256282109,18.4968000776565,-3.31124536858055));
#5055=CARTESIAN_POINT('Ctrl Pts',(-0.0593837235092786,18.6218000776565,
-3.68011778483394));
#5056=CARTESIAN_POINT('Ctrl Pts',(1.02784639780354,18.7468000776565,-3.34615024548552));
#5057=CARTESIAN_POINT('Ctrl Pts',(2.11507651911636,18.8718000776565,-3.01218270613711));
#5058=CARTESIAN_POINT('Ctrl Pts',(2.79836296968137,18.9968000776565,-2.10293946007882));
#5059=CARTESIAN_POINT('Ctrl Pts',(3.48164942024637,19.1218000776565,-1.19369621402054));
#5060=CARTESIAN_POINT('Ctrl Pts',(3.5,19.2468000776565,-0.0564772772053694));
#5061=CARTESIAN_POINT('Ctrl Pts',(3.51835057975363,19.3718000776565,1.0807416596098));
#5062=CARTESIAN_POINT('Ctrl Pts',(2.86475599094327,19.4968000776565,2.01155730596849));
#5063=CARTESIAN_POINT('Ctrl Pts',(2.2111614021329,19.6218000776565,2.94237295232717));
#5064=CARTESIAN_POINT('Ctrl Pts',(1.13527256282109,19.7468000776565,3.31124536858055));
#5065=CARTESIAN_POINT('Ctrl Pts',(0.0593837235092791,19.8718000776565,3.68011778483394));
#5066=CARTESIAN_POINT('Ctrl Pts',(-1.02784639780354,19.9968000776565,3.34615024548552));
#5067=CARTESIAN_POINT('Ctrl Pts',(-2.11507651911636,20.1218000776565,3.01218270613711));
#5068=CARTESIAN_POINT('Ctrl Pts',(-2.79836296968137,20.2468000776565,2.10293946007882));
#5069=CARTESIAN_POINT('Ctrl Pts',(-3.48164942024637,20.3718000776565,1.19369621402054));
#5070=CARTESIAN_POINT('Ctrl Pts',(-3.5,20.4968000776565,0.0564772772053689));
#5071=CARTESIAN_POINT('Ctrl Pts',(-3.51835057975363,20.6218000776565,-1.0807416596098));
#5072=CARTESIAN_POINT('Ctrl Pts',(-2.86475599094327,20.7468000776565,-2.01155730596849));
#5073=CARTESIAN_POINT('Ctrl Pts',(-2.2111614021329,20.8718000776565,-2.94237295232717));
#5074=CARTESIAN_POINT('Ctrl Pts',(-1.13527256282109,20.9968000776565,-3.31124536858055));
#5075=CARTESIAN_POINT('Ctrl Pts',(-0.0593837235092786,21.1218000776565,
-3.68011778483394));
#5076=CARTESIAN_POINT('Ctrl Pts',(1.02784639780354,21.2468000776565,-3.34615024548552));
#5077=CARTESIAN_POINT('Ctrl Pts',(2.11507651911636,21.3718000776565,-3.01218270613711));
#5078=CARTESIAN_POINT('Ctrl Pts',(2.79836296968137,21.4968000776565,-2.10293946007882));
#5079=CARTESIAN_POINT('Ctrl Pts',(3.48164942024637,21.6218000776565,-1.19369621402054));
#5080=CARTESIAN_POINT('Ctrl Pts',(3.5,21.7468000776565,-0.0564772772053694));
#5081=CARTESIAN_POINT('Ctrl Pts',(3.51835057975363,21.8718000776565,1.0807416596098));
#5082=CARTESIAN_POINT('Ctrl Pts',(2.86475599094327,21.9968000776565,2.01155730596849));
#5083=CARTESIAN_POINT('Ctrl Pts',(2.2111614021329,22.1218000776565,2.94237295232717));
#5084=CARTESIAN_POINT('Ctrl Pts',(1.13527256282109,22.2468000776565,3.31124536858055));
#5085=CARTESIAN_POINT('Ctrl Pts',(0.0593837235092791,22.3718000776565,3.68011778483394));
#5086=CARTESIAN_POINT('Ctrl Pts',(-1.02784639780354,22.4968000776565,3.34615024548552));
#5087=CARTESIAN_POINT('Ctrl Pts',(-2.11507651911636,22.6218000776565,3.01218270613711));
#5088=CARTESIAN_POINT('Ctrl Pts',(-2.79836296968137,22.7468000776565,2.10293946007882));
#5089=CARTESIAN_POINT('Ctrl Pts',(-3.48164942024637,22.8718000776565,1.19369621402054));
#5090=CARTESIAN_POINT('Ctrl Pts',(-3.5,22.9968000776565,0.0564772772053689));
#5091=CARTESIAN_POINT('Ctrl Pts',(-3.51835057975363,23.1218000776565,-1.0807416596098));
#5092=CARTESIAN_POINT('Ctrl Pts',(-2.86475599094327,23.2468000776565,-2.01155730596849));
#5093=CARTESIAN_POINT('Ctrl Pts',(-2.2111614021329,23.3718000776565,-2.94237295232717));
#5094=CARTESIAN_POINT('Ctrl Pts',(-1.13527256282109,23.4968000776565,-3.31124536858055));
#5095=CARTESIAN_POINT('Ctrl Pts',(-0.0593837235092786,23.6218000776565,
-3.68011778483394));
#5096=CARTESIAN_POINT('Ctrl Pts',(1.02784639780354,23.7468000776565,-3.34615024548552));
#5097=CARTESIAN_POINT('Ctrl Pts',(2.11507651911636,23.8718000776565,-3.01218270613711));
#5098=CARTESIAN_POINT('Ctrl Pts',(2.79836296968137,23.9968000776565,-2.10293946007882));
#5099=CARTESIAN_POINT('Ctrl Pts',(3.48164942024637,24.1218000776565,-1.19369621402054));
#5100=CARTESIAN_POINT('Ctrl Pts',(3.5,24.2468000776565,-0.0564772772053694));
#5101=CARTESIAN_POINT('Ctrl Pts',(3.51835057975363,24.3718000776565,1.0807416596098));
#5102=CARTESIAN_POINT('Ctrl Pts',(2.86475599094327,24.4968000776565,2.01155730596849));
#5103=CARTESIAN_POINT('Ctrl Pts',(2.2111614021329,24.6218000776565,2.94237295232717));
#5104=CARTESIAN_POINT('Ctrl Pts',(1.13527256282109,24.7468000776565,3.31124536858055));
#5105=CARTESIAN_POINT('Ctrl Pts',(0.0593837235092791,24.8718000776565,3.68011778483394));
#5106=CARTESIAN_POINT('Ctrl Pts',(-1.02784639780354,24.9968000776565,3.34615024548552));
#5107=CARTESIAN_POINT('Ctrl Pts',(-2.11507651911636,25.1218000776565,3.01218270613711));
#5108=CARTESIAN_POINT('Ctrl Pts',(-2.79836296968137,25.2468000776565,2.10293946007882));
#5109=CARTESIAN_POINT('Ctrl Pts',(-3.48164942024637,25.3718000776565,1.19369621402054));
#5110=CARTESIAN_POINT('Ctrl Pts',(-3.5,25.4968000776565,0.0564772772053689));
#5111=CARTESIAN_POINT('Ctrl Pts',(-3.51835057975363,25.6218000776565,-1.0807416596098));
#5112=CARTESIAN_POINT('Ctrl Pts',(-2.86475599094327,25.7468000776565,-2.01155730596849));
#5113=CARTESIAN_POINT('Ctrl Pts',(-2.2111614021329,25.8718000776565,-2.94237295232717));
#5114=CARTESIAN_POINT('Ctrl Pts',(-1.13527256282109,25.9968000776565,-3.31124536858055));
#5115=CARTESIAN_POINT('Ctrl Pts',(-0.0593837235092786,26.1218000776565,
-3.68011778483394));
#5116=CARTESIAN_POINT('Ctrl Pts',(1.02784639780354,26.2468000776565,-3.34615024548552));
#5117=CARTESIAN_POINT('Ctrl Pts',(2.11507651911636,26.3718000776565,-3.01218270613711));
#5118=CARTESIAN_POINT('Ctrl Pts',(2.79836296968137,26.4968000776565,-2.10293946007882));
#5119=CARTESIAN_POINT('Ctrl Pts',(3.48164942024637,26.6218000776565,-1.19369621402054));
#5120=CARTESIAN_POINT('Ctrl Pts',(3.5,26.7468000776565,-0.0564772772053694));
#5121=CARTESIAN_POINT('Ctrl Pts',(3.51835057975363,26.8718000776565,1.0807416596098));
#5122=CARTESIAN_POINT('Ctrl Pts',(2.86475599094327,26.9968000776565,2.01155730596849));
#5123=CARTESIAN_POINT('Ctrl Pts',(2.2111614021329,27.1218000776565,2.94237295232717));
#5124=CARTESIAN_POINT('Ctrl Pts',(1.13527256282109,27.2468000776565,3.31124536858055));
#5125=CARTESIAN_POINT('Ctrl Pts',(0.0593837235092791,27.3718000776565,3.68011778483394));
#5126=CARTESIAN_POINT('Ctrl Pts',(-1.02784639780354,27.4968000776565,3.34615024548552));
#5127=CARTESIAN_POINT('Ctrl Pts',(-2.11507651911636,27.6218000776565,3.01218270613711));
#5128=CARTESIAN_POINT('Ctrl Pts',(-2.79836296968137,27.7468000776565,2.10293946007882));
#5129=CARTESIAN_POINT('Ctrl Pts',(-3.48164942024637,27.8718000776565,1.19369621402054));
#5130=CARTESIAN_POINT('Ctrl Pts',(-3.5,27.9968000776565,0.0564772772053689));
#5131=CARTESIAN_POINT('Ctrl Pts',(-3.51835057975363,28.1218000776565,-1.0807416596098));
#5132=CARTESIAN_POINT('Ctrl Pts',(-2.86475599094327,28.2468000776565,-2.01155730596849));
#5133=CARTESIAN_POINT('Ctrl Pts',(-2.2111614021329,28.3718000776565,-2.94237295232717));
#5134=CARTESIAN_POINT('Ctrl Pts',(-1.13527256282109,28.4968000776565,-3.31124536858055));
#5135=CARTESIAN_POINT('Ctrl Pts',(-0.0593837235092786,28.6218000776565,
-3.68011778483394));
#5136=CARTESIAN_POINT('Ctrl Pts',(1.02784639780354,28.7468000776565,-3.34615024548552));
#5137=CARTESIAN_POINT('Ctrl Pts',(2.11507651911636,28.8718000776565,-3.01218270613711));
#5138=CARTESIAN_POINT('Ctrl Pts',(2.79836296968137,28.9968000776565,-2.10293946007882));
#5139=CARTESIAN_POINT('Ctrl Pts',(3.48164942024637,29.1218000776565,-1.19369621402054));
#5140=CARTESIAN_POINT('Ctrl Pts',(3.5,29.2468000776565,-0.0564772772053694));
#5141=CARTESIAN_POINT('Ctrl Pts',(3.51835057975363,29.3718000776565,1.0807416596098));
#5142=CARTESIAN_POINT('Ctrl Pts',(2.86475599094327,29.4968000776565,2.01155730596849));
#5143=CARTESIAN_POINT('Ctrl Pts',(2.2111614021329,29.6218000776565,2.94237295232717));
#5144=CARTESIAN_POINT('Ctrl Pts',(1.13527256282109,29.7468000776565,3.31124536858055));
#5145=CARTESIAN_POINT('Ctrl Pts',(0.0593837235092791,29.8718000776565,3.68011778483394));
#5146=CARTESIAN_POINT('Ctrl Pts',(-1.02784639780354,29.9968000776565,3.34615024548552));
#5147=CARTESIAN_POINT('Ctrl Pts',(-2.11507651911636,30.1218000776565,3.01218270613711));
#5148=CARTESIAN_POINT('Ctrl Pts',(-2.79836296968137,30.2468000776565,2.10293946007882));
#5149=CARTESIAN_POINT('Ctrl Pts',(-3.48164942024637,30.3718000776565,1.19369621402054));
#5150=CARTESIAN_POINT('Ctrl Pts',(-3.5,30.4968000776565,0.0564772772053689));
#5151=CARTESIAN_POINT('Ctrl Pts',(-3.51835057975363,30.6218000776565,-1.0807416596098));
#5152=CARTESIAN_POINT('Ctrl Pts',(-2.86475599094327,30.7468000776565,-2.01155730596849));
#5153=CARTESIAN_POINT('Ctrl Pts',(-2.2111614021329,30.8718000776565,-2.94237295232717));
#5154=CARTESIAN_POINT('Ctrl Pts',(-1.13527256282109,30.9968000776565,-3.31124536858055));
#5155=CARTESIAN_POINT('Ctrl Pts',(-0.0593837235092786,31.1218000776565,
-3.68011778483394));
#5156=CARTESIAN_POINT('Ctrl Pts',(1.02784639780354,31.2468000776565,-3.34615024548552));
#5157=CARTESIAN_POINT('Ctrl Pts',(2.11507651911636,31.3718000776565,-3.01218270613711));
#5158=CARTESIAN_POINT('Ctrl Pts',(2.79836296968137,31.4968000776565,-2.10293946007882));
#5159=CARTESIAN_POINT('Ctrl Pts',(3.48164942024637,31.6218000776565,-1.19369621402054));
#5160=CARTESIAN_POINT('Ctrl Pts',(3.5,31.7468000776565,-0.0564772772053694));
#5161=CARTESIAN_POINT('Ctrl Pts',(3.51835057975363,31.8718000776565,1.0807416596098));
#5162=CARTESIAN_POINT('Ctrl Pts',(2.86475599094327,31.9968000776565,2.01155730596849));
#5163=CARTESIAN_POINT('Ctrl Pts',(2.2111614021329,32.1218000776565,2.94237295232717));
#5164=CARTESIAN_POINT('Ctrl Pts',(1.13527256282109,32.2468000776565,3.31124536858055));
#5165=CARTESIAN_POINT('Ctrl Pts',(0.0593837235092791,32.3718000776565,3.68011778483394));
#5166=CARTESIAN_POINT('Ctrl Pts',(-1.02784639780354,32.4968000776565,3.34615024548552));
#5167=CARTESIAN_POINT('Ctrl Pts',(-2.11507651911636,32.6218000776565,3.01218270613711));
#5168=CARTESIAN_POINT('Ctrl Pts',(-2.79836296968137,32.7468000776565,2.10293946007882));
#5169=CARTESIAN_POINT('Ctrl Pts',(-3.48164942024637,32.8718000776565,1.19369621402054));
#5170=CARTESIAN_POINT('Ctrl Pts',(-3.5,32.9968000776565,0.0564772772053689));
#5171=CARTESIAN_POINT('Ctrl Pts',(-3.51835057975363,33.1218000776565,-1.0807416596098));
#5172=CARTESIAN_POINT('Ctrl Pts',(-2.86475599094327,33.2468000776565,-2.01155730596849));
#5173=CARTESIAN_POINT('Ctrl Pts',(-2.2111614021329,33.3718000776565,-2.94237295232717));
#5174=CARTESIAN_POINT('Ctrl Pts',(-1.13527256282109,33.4968000776565,-3.31124536858055));
#5175=CARTESIAN_POINT('Ctrl Pts',(-0.0593837235092786,33.6218000776565,
-3.68011778483394));
#5176=CARTESIAN_POINT('Ctrl Pts',(1.02784639780354,33.7468000776565,-3.34615024548552));
#5177=CARTESIAN_POINT('Ctrl Pts',(2.11507651911636,33.8718000776565,-3.01218270613711));
#5178=CARTESIAN_POINT('Ctrl Pts',(2.79836296968137,33.9968000776565,-2.10293946007882));
#5179=CARTESIAN_POINT('Ctrl Pts',(3.48164942024637,34.1218000776565,-1.19369621402054));
#5180=CARTESIAN_POINT('Ctrl Pts',(3.5,34.2468000776565,-0.0564772772053694));
#5181=CARTESIAN_POINT('Ctrl Pts',(3.51835057975363,34.3718000776565,1.0807416596098));
#5182=CARTESIAN_POINT('Ctrl Pts',(2.86475599094327,34.4968000776565,2.01155730596849));
#5183=CARTESIAN_POINT('Ctrl Pts',(2.2111614021329,34.6218000776565,2.94237295232717));
#5184=CARTESIAN_POINT('Ctrl Pts',(1.13527256282109,34.7468000776565,3.31124536858055));
#5185=CARTESIAN_POINT('Ctrl Pts',(0.0593837235092791,34.8718000776565,3.68011778483394));
#5186=CARTESIAN_POINT('Ctrl Pts',(-1.02784639780354,34.9968000776565,3.34615024548552));
#5187=CARTESIAN_POINT('Ctrl Pts',(-2.11507651911636,35.1218000776565,3.01218270613711));
#5188=CARTESIAN_POINT('Ctrl Pts',(-2.79836296968137,35.2468000776565,2.10293946007882));
#5189=CARTESIAN_POINT('Ctrl Pts',(-3.48164942024637,35.3718000776565,1.19369621402054));
#5190=CARTESIAN_POINT('Ctrl Pts',(-3.5,35.4968000776565,0.0564772772053689));
#5191=CARTESIAN_POINT('Ctrl Pts',(-3.51835057975363,35.6218000776565,-1.0807416596098));
#5192=CARTESIAN_POINT('Ctrl Pts',(-2.86475599094327,35.7468000776565,-2.01155730596849));
#5193=CARTESIAN_POINT('Ctrl Pts',(-2.2111614021329,35.8718000776565,-2.94237295232717));
#5194=CARTESIAN_POINT('Ctrl Pts',(-1.13527256282109,35.9968000776565,-3.31124536858055));
#5195=CARTESIAN_POINT('Ctrl Pts',(-0.0593837235092786,36.1218000776565,
-3.68011778483394));
#5196=CARTESIAN_POINT('Ctrl Pts',(1.02784639780354,36.2468000776565,-3.34615024548552));
#5197=CARTESIAN_POINT('Ctrl Pts',(2.11507651911636,36.3718000776565,-3.01218270613711));
#5198=CARTESIAN_POINT('Ctrl Pts',(2.79836296968137,36.4968000776565,-2.10293946007882));
#5199=CARTESIAN_POINT('Ctrl Pts',(3.48164942024637,36.6218000776565,-1.19369621402054));
#5200=CARTESIAN_POINT('Ctrl Pts',(3.5,36.7468000776565,-0.0564772772053694));
#5201=CARTESIAN_POINT('Ctrl Pts',(3.51835057975363,36.8718000776565,1.0807416596098));
#5202=CARTESIAN_POINT('Ctrl Pts',(2.86475599094327,36.9968000776565,2.01155730596849));
#5203=CARTESIAN_POINT('Ctrl Pts',(2.2111614021329,37.1218000776565,2.94237295232717));
#5204=CARTESIAN_POINT('Ctrl Pts',(1.13527256282109,37.2468000776565,3.31124536858055));
#5205=CARTESIAN_POINT('Ctrl Pts',(0.0593837235092791,37.3718000776565,3.68011778483394));
#5206=CARTESIAN_POINT('Ctrl Pts',(-1.02784639780354,37.4968000776565,3.34615024548552));
#5207=CARTESIAN_POINT('Ctrl Pts',(-2.11507651911636,37.6218000776565,3.01218270613711));
#5208=CARTESIAN_POINT('Ctrl Pts',(-2.79836296968137,37.7468000776565,2.10293946007882));
#5209=CARTESIAN_POINT('Ctrl Pts',(-3.48164942024637,37.8718000776565,1.19369621402054));
#5210=CARTESIAN_POINT('Ctrl Pts',(-3.5,37.9968000776565,0.0564772772053689));
#5211=CARTESIAN_POINT('Ctrl Pts',(-3.51835057975363,38.1218000776565,-1.0807416596098));
#5212=CARTESIAN_POINT('Ctrl Pts',(-2.86475599094327,38.2468000776565,-2.01155730596849));
#5213=CARTESIAN_POINT('Ctrl Pts',(-2.2111614021329,38.3718000776565,-2.94237295232717));
#5214=CARTESIAN_POINT('Ctrl Pts',(-1.13527256282109,38.4968000776565,-3.31124536858055));
#5215=CARTESIAN_POINT('Ctrl Pts',(-0.0593837235092786,38.6218000776565,
-3.68011778483394));
#5216=CARTESIAN_POINT('Ctrl Pts',(1.02784639780354,38.7468000776565,-3.34615024548552));
#5217=CARTESIAN_POINT('Ctrl Pts',(2.11507651911636,38.8718000776565,-3.01218270613711));
#5218=CARTESIAN_POINT('Ctrl Pts',(2.79836296968137,38.9968000776565,-2.10293946007882));
#5219=CARTESIAN_POINT('Ctrl Pts',(3.48164942024637,39.1218000776565,-1.19369621402054));
#5220=CARTESIAN_POINT('Ctrl Pts',(3.5,39.2468000776565,-0.0564772772053694));
#5221=CARTESIAN_POINT('Ctrl Pts',(3.51835057975363,39.3718000776565,1.0807416596098));
#5222=CARTESIAN_POINT('Ctrl Pts',(2.86475599094327,39.4968000776565,2.01155730596849));
#5223=CARTESIAN_POINT('Ctrl Pts',(2.2111614021329,39.6218000776565,2.94237295232717));
#5224=CARTESIAN_POINT('Ctrl Pts',(1.13527256282109,39.7468000776565,3.31124536858055));
#5225=CARTESIAN_POINT('Ctrl Pts',(0.0593837235092791,39.8718000776565,3.68011778483394));
#5226=CARTESIAN_POINT('Ctrl Pts',(-1.02784639780354,39.9968000776565,3.34615024548552));
#5227=CARTESIAN_POINT('Ctrl Pts',(-2.11507651911636,40.1218000776565,3.01218270613711));
#5228=CARTESIAN_POINT('Ctrl Pts',(-2.79836296968137,40.2468000776565,2.10293946007882));
#5229=CARTESIAN_POINT('Ctrl Pts',(-3.48164942024637,40.3718000776565,1.19369621402054));
#5230=CARTESIAN_POINT('Ctrl Pts',(-3.5,40.4968000776565,0.0564772772053689));
#5231=CARTESIAN_POINT('',(-1.05560584366888,15.,-3.33749696414134));
#5232=CARTESIAN_POINT('',(-3.,15.,3.04863211306834E-14));
#5233=CARTESIAN_POINT('Ctrl Pts',(-1.05560584366887,15.,-3.33749696414134));
#5234=CARTESIAN_POINT('Ctrl Pts',(-1.05394151307971,15.,-3.3325158524897));
#5235=CARTESIAN_POINT('Ctrl Pts',(-1.05302581964714,15.,-3.32739803279745));
#5236=CARTESIAN_POINT('Ctrl Pts',(-1.05250282072891,15.,-3.31638533458449));
#5237=CARTESIAN_POINT('Ctrl Pts',(-1.0530441514054,14.9999999999996,-3.31062365811979));
#5238=CARTESIAN_POINT('Ctrl Pts',(-1.05686193571968,14.9999999999996,-3.29147078572532));
#5239=CARTESIAN_POINT('Ctrl Pts',(-1.06302909045672,15.,-3.27779288376222));
#5240=CARTESIAN_POINT('Ctrl Pts',(-1.09049428069001,15.,-3.23176963091457));
#5241=CARTESIAN_POINT('Ctrl Pts',(-1.12473174639127,15.,-3.19498750811399));
#5242=CARTESIAN_POINT('Ctrl Pts',(-1.27982154446677,15.,-3.05221474570734));
#5243=CARTESIAN_POINT('Ctrl Pts',(-1.45769115884876,15.,-2.92194246708069));
#5244=CARTESIAN_POINT('Ctrl Pts',(-1.88593610007892,15.,-2.54883289900392));
#5245=CARTESIAN_POINT('Ctrl Pts',(-2.1703656445531,15.,-2.27198918349741));
#5246=CARTESIAN_POINT('Ctrl Pts',(-2.5725161275751,15.,-1.66624001122359));
#5247=CARTESIAN_POINT('Ctrl Pts',(-2.72305386070332,15.,-1.38777729550143));
#5248=CARTESIAN_POINT('Ctrl Pts',(-2.94442189004107,15.,-0.700038275746447));
#5249=CARTESIAN_POINT('Ctrl Pts',(-3.00000000000001,15.,-0.351019517027752));
#5250=CARTESIAN_POINT('Ctrl Pts',(-3.,15.,2.96464242044436E-14));
#5251=CARTESIAN_POINT('',(-3.5,39.5031999223435,-0.056477277205296));
#5252=CARTESIAN_POINT('Ctrl Pts',(-1.05560584366888,15.,-3.33749696414134));
#5253=CARTESIAN_POINT('Ctrl Pts',(-1.04174409073731,15.0016020898492,-3.34188125199396));
#5254=CARTESIAN_POINT('Ctrl Pts',(-1.02784639780361,15.0031999223435,-3.3461502454855));
#5255=CARTESIAN_POINT('Ctrl Pts',(0.0593837235092011,15.1281999223435,-3.68011778483394));
#5256=CARTESIAN_POINT('Ctrl Pts',(1.13527256282102,15.2531999223435,-3.31124536858058));
#5257=CARTESIAN_POINT('Ctrl Pts',(2.21116140213284,15.3781999223435,-2.94237295232722));
#5258=CARTESIAN_POINT('Ctrl Pts',(2.86475599094322,15.5031999223435,-2.01155730596855));
#5259=CARTESIAN_POINT('Ctrl Pts',(3.51835057975361,15.6281999223435,-1.08074165960988));
#5260=CARTESIAN_POINT('Ctrl Pts',(3.5,15.7531999223435,0.0564772772052952));
#5261=CARTESIAN_POINT('Ctrl Pts',(3.4816494202464,15.8781999223435,1.19369621402047));
#5262=CARTESIAN_POINT('Ctrl Pts',(2.79836296968141,16.0031999223435,2.10293946007876));
#5263=CARTESIAN_POINT('Ctrl Pts',(2.11507651911643,16.1281999223435,3.01218270613706));
#5264=CARTESIAN_POINT('Ctrl Pts',(1.02784639780361,16.2531999223435,3.3461502454855));
#5265=CARTESIAN_POINT('Ctrl Pts',(-0.0593837235092006,16.3781999223435,
3.68011778483394));
#5266=CARTESIAN_POINT('Ctrl Pts',(-1.13527256282102,16.5031999223435,3.31124536858058));
#5267=CARTESIAN_POINT('Ctrl Pts',(-2.21116140213284,16.6281999223435,2.94237295232722));
#5268=CARTESIAN_POINT('Ctrl Pts',(-2.86475599094322,16.7531999223435,2.01155730596855));
#5269=CARTESIAN_POINT('Ctrl Pts',(-3.51835057975361,16.8781999223435,1.08074165960988));
#5270=CARTESIAN_POINT('Ctrl Pts',(-3.5,17.0031999223435,-0.0564772772052956));
#5271=CARTESIAN_POINT('Ctrl Pts',(-3.4816494202464,17.1281999223435,-1.19369621402047));
#5272=CARTESIAN_POINT('Ctrl Pts',(-2.79836296968141,17.2531999223435,-2.10293946007877));
#5273=CARTESIAN_POINT('Ctrl Pts',(-2.11507651911643,17.3781999223435,-3.01218270613706));
#5274=CARTESIAN_POINT('Ctrl Pts',(-1.02784639780361,17.5031999223435,-3.3461502454855));
#5275=CARTESIAN_POINT('Ctrl Pts',(0.0593837235092011,17.6281999223435,-3.68011778483394));
#5276=CARTESIAN_POINT('Ctrl Pts',(1.13527256282102,17.7531999223435,-3.31124536858058));
#5277=CARTESIAN_POINT('Ctrl Pts',(2.21116140213284,17.8781999223435,-2.94237295232722));
#5278=CARTESIAN_POINT('Ctrl Pts',(2.86475599094322,18.0031999223435,-2.01155730596855));
#5279=CARTESIAN_POINT('Ctrl Pts',(3.51835057975361,18.1281999223435,-1.08074165960988));
#5280=CARTESIAN_POINT('Ctrl Pts',(3.5,18.2531999223435,0.0564772772052952));
#5281=CARTESIAN_POINT('Ctrl Pts',(3.4816494202464,18.3781999223435,1.19369621402047));
#5282=CARTESIAN_POINT('Ctrl Pts',(2.79836296968141,18.5031999223435,2.10293946007876));
#5283=CARTESIAN_POINT('Ctrl Pts',(2.11507651911643,18.6281999223435,3.01218270613706));
#5284=CARTESIAN_POINT('Ctrl Pts',(1.02784639780361,18.7531999223435,3.3461502454855));
#5285=CARTESIAN_POINT('Ctrl Pts',(-0.0593837235092006,18.8781999223435,
3.68011778483394));
#5286=CARTESIAN_POINT('Ctrl Pts',(-1.13527256282102,19.0031999223435,3.31124536858058));
#5287=CARTESIAN_POINT('Ctrl Pts',(-2.21116140213284,19.1281999223435,2.94237295232722));
#5288=CARTESIAN_POINT('Ctrl Pts',(-2.86475599094322,19.2531999223435,2.01155730596855));
#5289=CARTESIAN_POINT('Ctrl Pts',(-3.51835057975361,19.3781999223435,1.08074165960988));
#5290=CARTESIAN_POINT('Ctrl Pts',(-3.5,19.5031999223435,-0.0564772772052956));
#5291=CARTESIAN_POINT('Ctrl Pts',(-3.4816494202464,19.6281999223435,-1.19369621402047));
#5292=CARTESIAN_POINT('Ctrl Pts',(-2.79836296968141,19.7531999223435,-2.10293946007877));
#5293=CARTESIAN_POINT('Ctrl Pts',(-2.11507651911643,19.8781999223435,-3.01218270613706));
#5294=CARTESIAN_POINT('Ctrl Pts',(-1.02784639780361,20.0031999223435,-3.3461502454855));
#5295=CARTESIAN_POINT('Ctrl Pts',(0.0593837235092011,20.1281999223435,-3.68011778483394));
#5296=CARTESIAN_POINT('Ctrl Pts',(1.13527256282102,20.2531999223435,-3.31124536858058));
#5297=CARTESIAN_POINT('Ctrl Pts',(2.21116140213284,20.3781999223435,-2.94237295232722));
#5298=CARTESIAN_POINT('Ctrl Pts',(2.86475599094322,20.5031999223435,-2.01155730596855));
#5299=CARTESIAN_POINT('Ctrl Pts',(3.51835057975361,20.6281999223435,-1.08074165960988));
#5300=CARTESIAN_POINT('Ctrl Pts',(3.5,20.7531999223435,0.0564772772052952));
#5301=CARTESIAN_POINT('Ctrl Pts',(3.4816494202464,20.8781999223435,1.19369621402047));
#5302=CARTESIAN_POINT('Ctrl Pts',(2.79836296968141,21.0031999223435,2.10293946007876));
#5303=CARTESIAN_POINT('Ctrl Pts',(2.11507651911643,21.1281999223435,3.01218270613706));
#5304=CARTESIAN_POINT('Ctrl Pts',(1.02784639780361,21.2531999223435,3.3461502454855));
#5305=CARTESIAN_POINT('Ctrl Pts',(-0.0593837235092006,21.3781999223435,
3.68011778483394));
#5306=CARTESIAN_POINT('Ctrl Pts',(-1.13527256282102,21.5031999223435,3.31124536858058));
#5307=CARTESIAN_POINT('Ctrl Pts',(-2.21116140213284,21.6281999223435,2.94237295232722));
#5308=CARTESIAN_POINT('Ctrl Pts',(-2.86475599094322,21.7531999223435,2.01155730596855));
#5309=CARTESIAN_POINT('Ctrl Pts',(-3.51835057975361,21.8781999223435,1.08074165960988));
#5310=CARTESIAN_POINT('Ctrl Pts',(-3.5,22.0031999223435,-0.0564772772052956));
#5311=CARTESIAN_POINT('Ctrl Pts',(-3.4816494202464,22.1281999223435,-1.19369621402047));
#5312=CARTESIAN_POINT('Ctrl Pts',(-2.79836296968141,22.2531999223435,-2.10293946007877));
#5313=CARTESIAN_POINT('Ctrl Pts',(-2.11507651911643,22.3781999223435,-3.01218270613706));
#5314=CARTESIAN_POINT('Ctrl Pts',(-1.02784639780361,22.5031999223435,-3.3461502454855));
#5315=CARTESIAN_POINT('Ctrl Pts',(0.0593837235092011,22.6281999223435,-3.68011778483394));
#5316=CARTESIAN_POINT('Ctrl Pts',(1.13527256282102,22.7531999223435,-3.31124536858058));
#5317=CARTESIAN_POINT('Ctrl Pts',(2.21116140213284,22.8781999223435,-2.94237295232722));
#5318=CARTESIAN_POINT('Ctrl Pts',(2.86475599094322,23.0031999223435,-2.01155730596855));
#5319=CARTESIAN_POINT('Ctrl Pts',(3.51835057975361,23.1281999223435,-1.08074165960988));
#5320=CARTESIAN_POINT('Ctrl Pts',(3.5,23.2531999223435,0.0564772772052952));
#5321=CARTESIAN_POINT('Ctrl Pts',(3.4816494202464,23.3781999223435,1.19369621402047));
#5322=CARTESIAN_POINT('Ctrl Pts',(2.79836296968141,23.5031999223435,2.10293946007876));
#5323=CARTESIAN_POINT('Ctrl Pts',(2.11507651911643,23.6281999223435,3.01218270613706));
#5324=CARTESIAN_POINT('Ctrl Pts',(1.02784639780361,23.7531999223435,3.3461502454855));
#5325=CARTESIAN_POINT('Ctrl Pts',(-0.0593837235092006,23.8781999223435,
3.68011778483394));
#5326=CARTESIAN_POINT('Ctrl Pts',(-1.13527256282102,24.0031999223435,3.31124536858058));
#5327=CARTESIAN_POINT('Ctrl Pts',(-2.21116140213284,24.1281999223435,2.94237295232722));
#5328=CARTESIAN_POINT('Ctrl Pts',(-2.86475599094322,24.2531999223435,2.01155730596855));
#5329=CARTESIAN_POINT('Ctrl Pts',(-3.51835057975361,24.3781999223435,1.08074165960988));
#5330=CARTESIAN_POINT('Ctrl Pts',(-3.5,24.5031999223435,-0.0564772772052956));
#5331=CARTESIAN_POINT('Ctrl Pts',(-3.4816494202464,24.6281999223435,-1.19369621402047));
#5332=CARTESIAN_POINT('Ctrl Pts',(-2.79836296968141,24.7531999223435,-2.10293946007877));
#5333=CARTESIAN_POINT('Ctrl Pts',(-2.11507651911643,24.8781999223435,-3.01218270613706));
#5334=CARTESIAN_POINT('Ctrl Pts',(-1.02784639780361,25.0031999223435,-3.3461502454855));
#5335=CARTESIAN_POINT('Ctrl Pts',(0.0593837235092011,25.1281999223435,-3.68011778483394));
#5336=CARTESIAN_POINT('Ctrl Pts',(1.13527256282102,25.2531999223435,-3.31124536858058));
#5337=CARTESIAN_POINT('Ctrl Pts',(2.21116140213284,25.3781999223435,-2.94237295232722));
#5338=CARTESIAN_POINT('Ctrl Pts',(2.86475599094322,25.5031999223436,-2.01155730596855));
#5339=CARTESIAN_POINT('Ctrl Pts',(3.51835057975361,25.6281999223435,-1.08074165960988));
#5340=CARTESIAN_POINT('Ctrl Pts',(3.5,25.7531999223436,0.0564772772052952));
#5341=CARTESIAN_POINT('Ctrl Pts',(3.4816494202464,25.8781999223435,1.19369621402047));
#5342=CARTESIAN_POINT('Ctrl Pts',(2.79836296968141,26.0031999223435,2.10293946007876));
#5343=CARTESIAN_POINT('Ctrl Pts',(2.11507651911643,26.1281999223436,3.01218270613706));
#5344=CARTESIAN_POINT('Ctrl Pts',(1.02784639780361,26.2531999223435,3.3461502454855));
#5345=CARTESIAN_POINT('Ctrl Pts',(-0.0593837235092006,26.3781999223435,
3.68011778483394));
#5346=CARTESIAN_POINT('Ctrl Pts',(-1.13527256282102,26.5031999223435,3.31124536858058));
#5347=CARTESIAN_POINT('Ctrl Pts',(-2.21116140213284,26.6281999223435,2.94237295232722));
#5348=CARTESIAN_POINT('Ctrl Pts',(-2.86475599094322,26.7531999223436,2.01155730596855));
#5349=CARTESIAN_POINT('Ctrl Pts',(-3.51835057975361,26.8781999223435,1.08074165960988));
#5350=CARTESIAN_POINT('Ctrl Pts',(-3.5,27.0031999223436,-0.0564772772052956));
#5351=CARTESIAN_POINT('Ctrl Pts',(-3.4816494202464,27.1281999223435,-1.19369621402047));
#5352=CARTESIAN_POINT('Ctrl Pts',(-2.79836296968141,27.2531999223435,-2.10293946007877));
#5353=CARTESIAN_POINT('Ctrl Pts',(-2.11507651911643,27.3781999223436,-3.01218270613706));
#5354=CARTESIAN_POINT('Ctrl Pts',(-1.02784639780361,27.5031999223435,-3.3461502454855));
#5355=CARTESIAN_POINT('Ctrl Pts',(0.0593837235092011,27.6281999223435,-3.68011778483394));
#5356=CARTESIAN_POINT('Ctrl Pts',(1.13527256282102,27.7531999223435,-3.31124536858058));
#5357=CARTESIAN_POINT('Ctrl Pts',(2.21116140213284,27.8781999223435,-2.94237295232722));
#5358=CARTESIAN_POINT('Ctrl Pts',(2.86475599094322,28.0031999223435,-2.01155730596855));
#5359=CARTESIAN_POINT('Ctrl Pts',(3.51835057975361,28.1281999223435,-1.08074165960988));
#5360=CARTESIAN_POINT('Ctrl Pts',(3.5,28.2531999223435,0.0564772772052952));
#5361=CARTESIAN_POINT('Ctrl Pts',(3.4816494202464,28.3781999223435,1.19369621402047));
#5362=CARTESIAN_POINT('Ctrl Pts',(2.79836296968141,28.5031999223435,2.10293946007876));
#5363=CARTESIAN_POINT('Ctrl Pts',(2.11507651911643,28.6281999223435,3.01218270613706));
#5364=CARTESIAN_POINT('Ctrl Pts',(1.02784639780361,28.7531999223435,3.3461502454855));
#5365=CARTESIAN_POINT('Ctrl Pts',(-0.0593837235092006,28.8781999223435,
3.68011778483394));
#5366=CARTESIAN_POINT('Ctrl Pts',(-1.13527256282102,29.0031999223435,3.31124536858058));
#5367=CARTESIAN_POINT('Ctrl Pts',(-2.21116140213284,29.1281999223435,2.94237295232722));
#5368=CARTESIAN_POINT('Ctrl Pts',(-2.86475599094322,29.2531999223435,2.01155730596855));
#5369=CARTESIAN_POINT('Ctrl Pts',(-3.51835057975361,29.3781999223435,1.08074165960988));
#5370=CARTESIAN_POINT('Ctrl Pts',(-3.5,29.5031999223435,-0.0564772772052956));
#5371=CARTESIAN_POINT('Ctrl Pts',(-3.4816494202464,29.6281999223435,-1.19369621402047));
#5372=CARTESIAN_POINT('Ctrl Pts',(-2.79836296968141,29.7531999223435,-2.10293946007877));
#5373=CARTESIAN_POINT('Ctrl Pts',(-2.11507651911643,29.8781999223435,-3.01218270613706));
#5374=CARTESIAN_POINT('Ctrl Pts',(-1.02784639780361,30.0031999223435,-3.3461502454855));
#5375=CARTESIAN_POINT('Ctrl Pts',(0.0593837235092011,30.1281999223435,-3.68011778483394));
#5376=CARTESIAN_POINT('Ctrl Pts',(1.13527256282102,30.2531999223435,-3.31124536858058));
#5377=CARTESIAN_POINT('Ctrl Pts',(2.21116140213284,30.3781999223435,-2.94237295232722));
#5378=CARTESIAN_POINT('Ctrl Pts',(2.86475599094322,30.5031999223435,-2.01155730596855));
#5379=CARTESIAN_POINT('Ctrl Pts',(3.51835057975361,30.6281999223435,-1.08074165960988));
#5380=CARTESIAN_POINT('Ctrl Pts',(3.5,30.7531999223435,0.0564772772052952));
#5381=CARTESIAN_POINT('Ctrl Pts',(3.4816494202464,30.8781999223435,1.19369621402047));
#5382=CARTESIAN_POINT('Ctrl Pts',(2.79836296968141,31.0031999223435,2.10293946007876));
#5383=CARTESIAN_POINT('Ctrl Pts',(2.11507651911643,31.1281999223435,3.01218270613706));
#5384=CARTESIAN_POINT('Ctrl Pts',(1.02784639780361,31.2531999223435,3.3461502454855));
#5385=CARTESIAN_POINT('Ctrl Pts',(-0.0593837235092006,31.3781999223435,
3.68011778483394));
#5386=CARTESIAN_POINT('Ctrl Pts',(-1.13527256282102,31.5031999223435,3.31124536858058));
#5387=CARTESIAN_POINT('Ctrl Pts',(-2.21116140213284,31.6281999223435,2.94237295232722));
#5388=CARTESIAN_POINT('Ctrl Pts',(-2.86475599094322,31.7531999223435,2.01155730596855));
#5389=CARTESIAN_POINT('Ctrl Pts',(-3.51835057975361,31.8781999223435,1.08074165960988));
#5390=CARTESIAN_POINT('Ctrl Pts',(-3.5,32.0031999223435,-0.0564772772052956));
#5391=CARTESIAN_POINT('Ctrl Pts',(-3.4816494202464,32.1281999223435,-1.19369621402047));
#5392=CARTESIAN_POINT('Ctrl Pts',(-2.79836296968141,32.2531999223435,-2.10293946007877));
#5393=CARTESIAN_POINT('Ctrl Pts',(-2.11507651911643,32.3781999223436,-3.01218270613706));
#5394=CARTESIAN_POINT('Ctrl Pts',(-1.02784639780361,32.5031999223435,-3.3461502454855));
#5395=CARTESIAN_POINT('Ctrl Pts',(0.0593837235092011,32.6281999223435,-3.68011778483394));
#5396=CARTESIAN_POINT('Ctrl Pts',(1.13527256282102,32.7531999223435,-3.31124536858058));
#5397=CARTESIAN_POINT('Ctrl Pts',(2.21116140213284,32.8781999223435,-2.94237295232722));
#5398=CARTESIAN_POINT('Ctrl Pts',(2.86475599094322,33.0031999223436,-2.01155730596855));
#5399=CARTESIAN_POINT('Ctrl Pts',(3.51835057975361,33.1281999223435,-1.08074165960988));
#5400=CARTESIAN_POINT('Ctrl Pts',(3.5,33.2531999223435,0.0564772772052952));
#5401=CARTESIAN_POINT('Ctrl Pts',(3.4816494202464,33.3781999223435,1.19369621402047));
#5402=CARTESIAN_POINT('Ctrl Pts',(2.79836296968141,33.5031999223435,2.10293946007876));
#5403=CARTESIAN_POINT('Ctrl Pts',(2.11507651911643,33.6281999223435,3.01218270613706));
#5404=CARTESIAN_POINT('Ctrl Pts',(1.02784639780361,33.7531999223435,3.3461502454855));
#5405=CARTESIAN_POINT('Ctrl Pts',(-0.0593837235092006,33.8781999223435,
3.68011778483394));
#5406=CARTESIAN_POINT('Ctrl Pts',(-1.13527256282102,34.0031999223435,3.31124536858058));
#5407=CARTESIAN_POINT('Ctrl Pts',(-2.21116140213284,34.1281999223435,2.94237295232722));
#5408=CARTESIAN_POINT('Ctrl Pts',(-2.86475599094322,34.2531999223436,2.01155730596855));
#5409=CARTESIAN_POINT('Ctrl Pts',(-3.51835057975361,34.3781999223435,1.08074165960988));
#5410=CARTESIAN_POINT('Ctrl Pts',(-3.5,34.5031999223435,-0.0564772772052956));
#5411=CARTESIAN_POINT('Ctrl Pts',(-3.4816494202464,34.6281999223435,-1.19369621402047));
#5412=CARTESIAN_POINT('Ctrl Pts',(-2.79836296968141,34.7531999223435,-2.10293946007877));
#5413=CARTESIAN_POINT('Ctrl Pts',(-2.11507651911643,34.8781999223436,-3.01218270613706));
#5414=CARTESIAN_POINT('Ctrl Pts',(-1.02784639780361,35.0031999223435,-3.3461502454855));
#5415=CARTESIAN_POINT('Ctrl Pts',(0.0593837235092011,35.1281999223435,-3.68011778483394));
#5416=CARTESIAN_POINT('Ctrl Pts',(1.13527256282102,35.2531999223435,-3.31124536858058));
#5417=CARTESIAN_POINT('Ctrl Pts',(2.21116140213284,35.3781999223435,-2.94237295232722));
#5418=CARTESIAN_POINT('Ctrl Pts',(2.86475599094322,35.5031999223436,-2.01155730596855));
#5419=CARTESIAN_POINT('Ctrl Pts',(3.51835057975361,35.6281999223435,-1.08074165960988));
#5420=CARTESIAN_POINT('Ctrl Pts',(3.5,35.7531999223435,0.0564772772052952));
#5421=CARTESIAN_POINT('Ctrl Pts',(3.4816494202464,35.8781999223435,1.19369621402047));
#5422=CARTESIAN_POINT('Ctrl Pts',(2.79836296968141,36.0031999223435,2.10293946007876));
#5423=CARTESIAN_POINT('Ctrl Pts',(2.11507651911643,36.1281999223436,3.01218270613706));
#5424=CARTESIAN_POINT('Ctrl Pts',(1.02784639780361,36.2531999223435,3.3461502454855));
#5425=CARTESIAN_POINT('Ctrl Pts',(-0.0593837235092006,36.3781999223435,
3.68011778483394));
#5426=CARTESIAN_POINT('Ctrl Pts',(-1.13527256282102,36.5031999223435,3.31124536858058));
#5427=CARTESIAN_POINT('Ctrl Pts',(-2.21116140213284,36.6281999223435,2.94237295232722));
#5428=CARTESIAN_POINT('Ctrl Pts',(-2.86475599094322,36.7531999223435,2.01155730596855));
#5429=CARTESIAN_POINT('Ctrl Pts',(-3.51835057975361,36.8781999223435,1.08074165960988));
#5430=CARTESIAN_POINT('Ctrl Pts',(-3.5,37.0031999223435,-0.0564772772052956));
#5431=CARTESIAN_POINT('Ctrl Pts',(-3.4816494202464,37.1281999223435,-1.19369621402047));
#5432=CARTESIAN_POINT('Ctrl Pts',(-2.79836296968141,37.2531999223435,-2.10293946007877));
#5433=CARTESIAN_POINT('Ctrl Pts',(-2.11507651911643,37.3781999223435,-3.01218270613706));
#5434=CARTESIAN_POINT('Ctrl Pts',(-1.02784639780361,37.5031999223435,-3.3461502454855));
#5435=CARTESIAN_POINT('Ctrl Pts',(0.0593837235092011,37.6281999223435,-3.68011778483394));
#5436=CARTESIAN_POINT('Ctrl Pts',(1.13527256282102,37.7531999223435,-3.31124536858058));
#5437=CARTESIAN_POINT('Ctrl Pts',(2.21116140213284,37.8781999223435,-2.94237295232722));
#5438=CARTESIAN_POINT('Ctrl Pts',(2.86475599094322,38.0031999223435,-2.01155730596855));
#5439=CARTESIAN_POINT('Ctrl Pts',(3.51835057975361,38.1281999223435,-1.08074165960988));
#5440=CARTESIAN_POINT('Ctrl Pts',(3.5,38.2531999223435,0.0564772772052952));
#5441=CARTESIAN_POINT('Ctrl Pts',(3.4816494202464,38.3781999223435,1.19369621402047));
#5442=CARTESIAN_POINT('Ctrl Pts',(2.79836296968141,38.5031999223435,2.10293946007876));
#5443=CARTESIAN_POINT('Ctrl Pts',(2.11507651911643,38.6281999223435,3.01218270613706));
#5444=CARTESIAN_POINT('Ctrl Pts',(1.02784639780361,38.7531999223435,3.3461502454855));
#5445=CARTESIAN_POINT('Ctrl Pts',(-0.0593837235092006,38.8781999223435,
3.68011778483394));
#5446=CARTESIAN_POINT('Ctrl Pts',(-1.13527256282102,39.0031999223435,3.31124536858058));
#5447=CARTESIAN_POINT('Ctrl Pts',(-2.21116140213284,39.1281999223435,2.94237295232722));
#5448=CARTESIAN_POINT('Ctrl Pts',(-2.86475599094322,39.2531999223436,2.01155730596855));
#5449=CARTESIAN_POINT('Ctrl Pts',(-3.51835057975361,39.3781999223435,1.08074165960988));
#5450=CARTESIAN_POINT('Ctrl Pts',(-3.5,39.5031999223435,-0.056477277205296));
#5451=CARTESIAN_POINT('',(-3.5,40.4968000776565,0.0564772772053685));
#5452=CARTESIAN_POINT('Origin',(-3.5,40.,3.664603343001E-14));
#5453=CARTESIAN_POINT('',(-3.5,15.4968000776565,0.056477277205369));
#5454=CARTESIAN_POINT('Ctrl Pts',(-3.5,15.4968000776565,0.056477277205369));
#5455=CARTESIAN_POINT('Ctrl Pts',(-3.51835057975363,15.6218000776565,-1.0807416596098));
#5456=CARTESIAN_POINT('Ctrl Pts',(-2.86475599094327,15.7468000776565,-2.01155730596849));
#5457=CARTESIAN_POINT('Ctrl Pts',(-2.2111614021329,15.8718000776565,-2.94237295232717));
#5458=CARTESIAN_POINT('Ctrl Pts',(-1.13527256282109,15.9968000776565,-3.31124536858055));
#5459=CARTESIAN_POINT('Ctrl Pts',(-0.0593837235092786,16.1218000776565,
-3.68011778483394));
#5460=CARTESIAN_POINT('Ctrl Pts',(1.02784639780354,16.2468000776565,-3.34615024548552));
#5461=CARTESIAN_POINT('Ctrl Pts',(2.11507651911636,16.3718000776565,-3.01218270613711));
#5462=CARTESIAN_POINT('Ctrl Pts',(2.79836296968137,16.4968000776565,-2.10293946007882));
#5463=CARTESIAN_POINT('Ctrl Pts',(3.48164942024637,16.6218000776565,-1.19369621402054));
#5464=CARTESIAN_POINT('Ctrl Pts',(3.5,16.7468000776565,-0.0564772772053694));
#5465=CARTESIAN_POINT('Ctrl Pts',(3.51835057975363,16.8718000776565,1.0807416596098));
#5466=CARTESIAN_POINT('Ctrl Pts',(2.86475599094327,16.9968000776565,2.01155730596849));
#5467=CARTESIAN_POINT('Ctrl Pts',(2.2111614021329,17.1218000776565,2.94237295232717));
#5468=CARTESIAN_POINT('Ctrl Pts',(1.13527256282109,17.2468000776565,3.31124536858055));
#5469=CARTESIAN_POINT('Ctrl Pts',(0.0593837235092791,17.3718000776565,3.68011778483394));
#5470=CARTESIAN_POINT('Ctrl Pts',(-1.02784639780354,17.4968000776565,3.34615024548552));
#5471=CARTESIAN_POINT('Ctrl Pts',(-2.11507651911636,17.6218000776565,3.01218270613711));
#5472=CARTESIAN_POINT('Ctrl Pts',(-2.79836296968137,17.7468000776565,2.10293946007882));
#5473=CARTESIAN_POINT('Ctrl Pts',(-3.48164942024637,17.8718000776565,1.19369621402054));
#5474=CARTESIAN_POINT('Ctrl Pts',(-3.5,17.9968000776565,0.0564772772053689));
#5475=CARTESIAN_POINT('Ctrl Pts',(-3.51835057975363,18.1218000776565,-1.0807416596098));
#5476=CARTESIAN_POINT('Ctrl Pts',(-2.86475599094327,18.2468000776565,-2.01155730596849));
#5477=CARTESIAN_POINT('Ctrl Pts',(-2.2111614021329,18.3718000776565,-2.94237295232717));
#5478=CARTESIAN_POINT('Ctrl Pts',(-1.13527256282109,18.4968000776565,-3.31124536858055));
#5479=CARTESIAN_POINT('Ctrl Pts',(-0.0593837235092786,18.6218000776565,
-3.68011778483394));
#5480=CARTESIAN_POINT('Ctrl Pts',(1.02784639780354,18.7468000776565,-3.34615024548552));
#5481=CARTESIAN_POINT('Ctrl Pts',(2.11507651911636,18.8718000776565,-3.01218270613711));
#5482=CARTESIAN_POINT('Ctrl Pts',(2.79836296968137,18.9968000776565,-2.10293946007882));
#5483=CARTESIAN_POINT('Ctrl Pts',(3.48164942024637,19.1218000776565,-1.19369621402054));
#5484=CARTESIAN_POINT('Ctrl Pts',(3.5,19.2468000776565,-0.0564772772053694));
#5485=CARTESIAN_POINT('Ctrl Pts',(3.51835057975363,19.3718000776565,1.0807416596098));
#5486=CARTESIAN_POINT('Ctrl Pts',(2.86475599094327,19.4968000776565,2.01155730596849));
#5487=CARTESIAN_POINT('Ctrl Pts',(2.2111614021329,19.6218000776565,2.94237295232717));
#5488=CARTESIAN_POINT('Ctrl Pts',(1.13527256282109,19.7468000776565,3.31124536858055));
#5489=CARTESIAN_POINT('Ctrl Pts',(0.0593837235092791,19.8718000776565,3.68011778483394));
#5490=CARTESIAN_POINT('Ctrl Pts',(-1.02784639780354,19.9968000776565,3.34615024548552));
#5491=CARTESIAN_POINT('Ctrl Pts',(-2.11507651911636,20.1218000776565,3.01218270613711));
#5492=CARTESIAN_POINT('Ctrl Pts',(-2.79836296968137,20.2468000776565,2.10293946007882));
#5493=CARTESIAN_POINT('Ctrl Pts',(-3.48164942024637,20.3718000776565,1.19369621402054));
#5494=CARTESIAN_POINT('Ctrl Pts',(-3.5,20.4968000776565,0.0564772772053689));
#5495=CARTESIAN_POINT('Ctrl Pts',(-3.51835057975363,20.6218000776565,-1.0807416596098));
#5496=CARTESIAN_POINT('Ctrl Pts',(-2.86475599094327,20.7468000776565,-2.01155730596849));
#5497=CARTESIAN_POINT('Ctrl Pts',(-2.2111614021329,20.8718000776565,-2.94237295232717));
#5498=CARTESIAN_POINT('Ctrl Pts',(-1.13527256282109,20.9968000776565,-3.31124536858055));
#5499=CARTESIAN_POINT('Ctrl Pts',(-0.0593837235092786,21.1218000776565,
-3.68011778483394));
#5500=CARTESIAN_POINT('Ctrl Pts',(1.02784639780354,21.2468000776565,-3.34615024548552));
#5501=CARTESIAN_POINT('Ctrl Pts',(2.11507651911636,21.3718000776565,-3.01218270613711));
#5502=CARTESIAN_POINT('Ctrl Pts',(2.79836296968137,21.4968000776565,-2.10293946007882));
#5503=CARTESIAN_POINT('Ctrl Pts',(3.48164942024637,21.6218000776565,-1.19369621402054));
#5504=CARTESIAN_POINT('Ctrl Pts',(3.5,21.7468000776565,-0.0564772772053694));
#5505=CARTESIAN_POINT('Ctrl Pts',(3.51835057975363,21.8718000776565,1.0807416596098));
#5506=CARTESIAN_POINT('Ctrl Pts',(2.86475599094327,21.9968000776565,2.01155730596849));
#5507=CARTESIAN_POINT('Ctrl Pts',(2.2111614021329,22.1218000776565,2.94237295232717));
#5508=CARTESIAN_POINT('Ctrl Pts',(1.13527256282109,22.2468000776565,3.31124536858055));
#5509=CARTESIAN_POINT('Ctrl Pts',(0.0593837235092791,22.3718000776565,3.68011778483394));
#5510=CARTESIAN_POINT('Ctrl Pts',(-1.02784639780354,22.4968000776565,3.34615024548552));
#5511=CARTESIAN_POINT('Ctrl Pts',(-2.11507651911636,22.6218000776565,3.01218270613711));
#5512=CARTESIAN_POINT('Ctrl Pts',(-2.79836296968137,22.7468000776565,2.10293946007882));
#5513=CARTESIAN_POINT('Ctrl Pts',(-3.48164942024637,22.8718000776565,1.19369621402054));
#5514=CARTESIAN_POINT('Ctrl Pts',(-3.5,22.9968000776565,0.0564772772053689));
#5515=CARTESIAN_POINT('Ctrl Pts',(-3.51835057975363,23.1218000776565,-1.0807416596098));
#5516=CARTESIAN_POINT('Ctrl Pts',(-2.86475599094327,23.2468000776565,-2.01155730596849));
#5517=CARTESIAN_POINT('Ctrl Pts',(-2.2111614021329,23.3718000776565,-2.94237295232717));
#5518=CARTESIAN_POINT('Ctrl Pts',(-1.13527256282109,23.4968000776565,-3.31124536858055));
#5519=CARTESIAN_POINT('Ctrl Pts',(-0.0593837235092786,23.6218000776565,
-3.68011778483394));
#5520=CARTESIAN_POINT('Ctrl Pts',(1.02784639780354,23.7468000776565,-3.34615024548552));
#5521=CARTESIAN_POINT('Ctrl Pts',(2.11507651911636,23.8718000776565,-3.01218270613711));
#5522=CARTESIAN_POINT('Ctrl Pts',(2.79836296968137,23.9968000776565,-2.10293946007882));
#5523=CARTESIAN_POINT('Ctrl Pts',(3.48164942024637,24.1218000776565,-1.19369621402054));
#5524=CARTESIAN_POINT('Ctrl Pts',(3.5,24.2468000776565,-0.0564772772053694));
#5525=CARTESIAN_POINT('Ctrl Pts',(3.51835057975363,24.3718000776565,1.0807416596098));
#5526=CARTESIAN_POINT('Ctrl Pts',(2.86475599094327,24.4968000776565,2.01155730596849));
#5527=CARTESIAN_POINT('Ctrl Pts',(2.2111614021329,24.6218000776565,2.94237295232717));
#5528=CARTESIAN_POINT('Ctrl Pts',(1.13527256282109,24.7468000776565,3.31124536858055));
#5529=CARTESIAN_POINT('Ctrl Pts',(0.0593837235092791,24.8718000776565,3.68011778483394));
#5530=CARTESIAN_POINT('Ctrl Pts',(-1.02784639780354,24.9968000776565,3.34615024548552));
#5531=CARTESIAN_POINT('Ctrl Pts',(-2.11507651911636,25.1218000776565,3.01218270613711));
#5532=CARTESIAN_POINT('Ctrl Pts',(-2.79836296968137,25.2468000776565,2.10293946007882));
#5533=CARTESIAN_POINT('Ctrl Pts',(-3.48164942024637,25.3718000776565,1.19369621402054));
#5534=CARTESIAN_POINT('Ctrl Pts',(-3.5,25.4968000776565,0.0564772772053689));
#5535=CARTESIAN_POINT('Ctrl Pts',(-3.51835057975363,25.6218000776565,-1.0807416596098));
#5536=CARTESIAN_POINT('Ctrl Pts',(-2.86475599094327,25.7468000776565,-2.01155730596849));
#5537=CARTESIAN_POINT('Ctrl Pts',(-2.2111614021329,25.8718000776565,-2.94237295232717));
#5538=CARTESIAN_POINT('Ctrl Pts',(-1.13527256282109,25.9968000776565,-3.31124536858055));
#5539=CARTESIAN_POINT('Ctrl Pts',(-0.0593837235092786,26.1218000776565,
-3.68011778483394));
#5540=CARTESIAN_POINT('Ctrl Pts',(1.02784639780354,26.2468000776565,-3.34615024548552));
#5541=CARTESIAN_POINT('Ctrl Pts',(2.11507651911636,26.3718000776565,-3.01218270613711));
#5542=CARTESIAN_POINT('Ctrl Pts',(2.79836296968137,26.4968000776565,-2.10293946007882));
#5543=CARTESIAN_POINT('Ctrl Pts',(3.48164942024637,26.6218000776565,-1.19369621402054));
#5544=CARTESIAN_POINT('Ctrl Pts',(3.5,26.7468000776565,-0.0564772772053694));
#5545=CARTESIAN_POINT('Ctrl Pts',(3.51835057975363,26.8718000776565,1.0807416596098));
#5546=CARTESIAN_POINT('Ctrl Pts',(2.86475599094327,26.9968000776565,2.01155730596849));
#5547=CARTESIAN_POINT('Ctrl Pts',(2.2111614021329,27.1218000776565,2.94237295232717));
#5548=CARTESIAN_POINT('Ctrl Pts',(1.13527256282109,27.2468000776565,3.31124536858055));
#5549=CARTESIAN_POINT('Ctrl Pts',(0.0593837235092791,27.3718000776565,3.68011778483394));
#5550=CARTESIAN_POINT('Ctrl Pts',(-1.02784639780354,27.4968000776565,3.34615024548552));
#5551=CARTESIAN_POINT('Ctrl Pts',(-2.11507651911636,27.6218000776565,3.01218270613711));
#5552=CARTESIAN_POINT('Ctrl Pts',(-2.79836296968137,27.7468000776565,2.10293946007882));
#5553=CARTESIAN_POINT('Ctrl Pts',(-3.48164942024637,27.8718000776565,1.19369621402054));
#5554=CARTESIAN_POINT('Ctrl Pts',(-3.5,27.9968000776565,0.0564772772053689));
#5555=CARTESIAN_POINT('Ctrl Pts',(-3.51835057975363,28.1218000776565,-1.0807416596098));
#5556=CARTESIAN_POINT('Ctrl Pts',(-2.86475599094327,28.2468000776565,-2.01155730596849));
#5557=CARTESIAN_POINT('Ctrl Pts',(-2.2111614021329,28.3718000776565,-2.94237295232717));
#5558=CARTESIAN_POINT('Ctrl Pts',(-1.13527256282109,28.4968000776565,-3.31124536858055));
#5559=CARTESIAN_POINT('Ctrl Pts',(-0.0593837235092786,28.6218000776565,
-3.68011778483394));
#5560=CARTESIAN_POINT('Ctrl Pts',(1.02784639780354,28.7468000776565,-3.34615024548552));
#5561=CARTESIAN_POINT('Ctrl Pts',(2.11507651911636,28.8718000776565,-3.01218270613711));
#5562=CARTESIAN_POINT('Ctrl Pts',(2.79836296968137,28.9968000776565,-2.10293946007882));
#5563=CARTESIAN_POINT('Ctrl Pts',(3.48164942024637,29.1218000776565,-1.19369621402054));
#5564=CARTESIAN_POINT('Ctrl Pts',(3.5,29.2468000776565,-0.0564772772053694));
#5565=CARTESIAN_POINT('Ctrl Pts',(3.51835057975363,29.3718000776565,1.0807416596098));
#5566=CARTESIAN_POINT('Ctrl Pts',(2.86475599094327,29.4968000776565,2.01155730596849));
#5567=CARTESIAN_POINT('Ctrl Pts',(2.2111614021329,29.6218000776565,2.94237295232717));
#5568=CARTESIAN_POINT('Ctrl Pts',(1.13527256282109,29.7468000776565,3.31124536858055));
#5569=CARTESIAN_POINT('Ctrl Pts',(0.0593837235092791,29.8718000776565,3.68011778483394));
#5570=CARTESIAN_POINT('Ctrl Pts',(-1.02784639780354,29.9968000776565,3.34615024548552));
#5571=CARTESIAN_POINT('Ctrl Pts',(-2.11507651911636,30.1218000776565,3.01218270613711));
#5572=CARTESIAN_POINT('Ctrl Pts',(-2.79836296968137,30.2468000776565,2.10293946007882));
#5573=CARTESIAN_POINT('Ctrl Pts',(-3.48164942024637,30.3718000776565,1.19369621402054));
#5574=CARTESIAN_POINT('Ctrl Pts',(-3.5,30.4968000776565,0.0564772772053689));
#5575=CARTESIAN_POINT('Ctrl Pts',(-3.51835057975363,30.6218000776565,-1.0807416596098));
#5576=CARTESIAN_POINT('Ctrl Pts',(-2.86475599094327,30.7468000776565,-2.01155730596849));
#5577=CARTESIAN_POINT('Ctrl Pts',(-2.2111614021329,30.8718000776565,-2.94237295232717));
#5578=CARTESIAN_POINT('Ctrl Pts',(-1.13527256282109,30.9968000776565,-3.31124536858055));
#5579=CARTESIAN_POINT('Ctrl Pts',(-0.0593837235092786,31.1218000776565,
-3.68011778483394));
#5580=CARTESIAN_POINT('Ctrl Pts',(1.02784639780354,31.2468000776565,-3.34615024548552));
#5581=CARTESIAN_POINT('Ctrl Pts',(2.11507651911636,31.3718000776565,-3.01218270613711));
#5582=CARTESIAN_POINT('Ctrl Pts',(2.79836296968137,31.4968000776565,-2.10293946007882));
#5583=CARTESIAN_POINT('Ctrl Pts',(3.48164942024637,31.6218000776565,-1.19369621402054));
#5584=CARTESIAN_POINT('Ctrl Pts',(3.5,31.7468000776565,-0.0564772772053694));
#5585=CARTESIAN_POINT('Ctrl Pts',(3.51835057975363,31.8718000776565,1.0807416596098));
#5586=CARTESIAN_POINT('Ctrl Pts',(2.86475599094327,31.9968000776565,2.01155730596849));
#5587=CARTESIAN_POINT('Ctrl Pts',(2.2111614021329,32.1218000776565,2.94237295232717));
#5588=CARTESIAN_POINT('Ctrl Pts',(1.13527256282109,32.2468000776565,3.31124536858055));
#5589=CARTESIAN_POINT('Ctrl Pts',(0.0593837235092791,32.3718000776565,3.68011778483394));
#5590=CARTESIAN_POINT('Ctrl Pts',(-1.02784639780354,32.4968000776565,3.34615024548552));
#5591=CARTESIAN_POINT('Ctrl Pts',(-2.11507651911636,32.6218000776565,3.01218270613711));
#5592=CARTESIAN_POINT('Ctrl Pts',(-2.79836296968137,32.7468000776565,2.10293946007882));
#5593=CARTESIAN_POINT('Ctrl Pts',(-3.48164942024637,32.8718000776565,1.19369621402054));
#5594=CARTESIAN_POINT('Ctrl Pts',(-3.5,32.9968000776565,0.0564772772053689));
#5595=CARTESIAN_POINT('Ctrl Pts',(-3.51835057975363,33.1218000776565,-1.0807416596098));
#5596=CARTESIAN_POINT('Ctrl Pts',(-2.86475599094327,33.2468000776565,-2.01155730596849));
#5597=CARTESIAN_POINT('Ctrl Pts',(-2.2111614021329,33.3718000776565,-2.94237295232717));
#5598=CARTESIAN_POINT('Ctrl Pts',(-1.13527256282109,33.4968000776565,-3.31124536858055));
#5599=CARTESIAN_POINT('Ctrl Pts',(-0.0593837235092786,33.6218000776565,
-3.68011778483394));
#5600=CARTESIAN_POINT('Ctrl Pts',(1.02784639780354,33.7468000776565,-3.34615024548552));
#5601=CARTESIAN_POINT('Ctrl Pts',(2.11507651911636,33.8718000776565,-3.01218270613711));
#5602=CARTESIAN_POINT('Ctrl Pts',(2.79836296968137,33.9968000776565,-2.10293946007882));
#5603=CARTESIAN_POINT('Ctrl Pts',(3.48164942024637,34.1218000776565,-1.19369621402054));
#5604=CARTESIAN_POINT('Ctrl Pts',(3.5,34.2468000776565,-0.0564772772053694));
#5605=CARTESIAN_POINT('Ctrl Pts',(3.51835057975363,34.3718000776565,1.0807416596098));
#5606=CARTESIAN_POINT('Ctrl Pts',(2.86475599094327,34.4968000776565,2.01155730596849));
#5607=CARTESIAN_POINT('Ctrl Pts',(2.2111614021329,34.6218000776565,2.94237295232717));
#5608=CARTESIAN_POINT('Ctrl Pts',(1.13527256282109,34.7468000776565,3.31124536858055));
#5609=CARTESIAN_POINT('Ctrl Pts',(0.0593837235092791,34.8718000776565,3.68011778483394));
#5610=CARTESIAN_POINT('Ctrl Pts',(-1.02784639780354,34.9968000776565,3.34615024548552));
#5611=CARTESIAN_POINT('Ctrl Pts',(-2.11507651911636,35.1218000776565,3.01218270613711));
#5612=CARTESIAN_POINT('Ctrl Pts',(-2.79836296968137,35.2468000776565,2.10293946007882));
#5613=CARTESIAN_POINT('Ctrl Pts',(-3.48164942024637,35.3718000776565,1.19369621402054));
#5614=CARTESIAN_POINT('Ctrl Pts',(-3.5,35.4968000776565,0.0564772772053689));
#5615=CARTESIAN_POINT('Ctrl Pts',(-3.51835057975363,35.6218000776565,-1.0807416596098));
#5616=CARTESIAN_POINT('Ctrl Pts',(-2.86475599094327,35.7468000776565,-2.01155730596849));
#5617=CARTESIAN_POINT('Ctrl Pts',(-2.2111614021329,35.8718000776565,-2.94237295232717));
#5618=CARTESIAN_POINT('Ctrl Pts',(-1.13527256282109,35.9968000776565,-3.31124536858055));
#5619=CARTESIAN_POINT('Ctrl Pts',(-0.0593837235092786,36.1218000776565,
-3.68011778483394));
#5620=CARTESIAN_POINT('Ctrl Pts',(1.02784639780354,36.2468000776565,-3.34615024548552));
#5621=CARTESIAN_POINT('Ctrl Pts',(2.11507651911636,36.3718000776565,-3.01218270613711));
#5622=CARTESIAN_POINT('Ctrl Pts',(2.79836296968137,36.4968000776565,-2.10293946007882));
#5623=CARTESIAN_POINT('Ctrl Pts',(3.48164942024637,36.6218000776565,-1.19369621402054));
#5624=CARTESIAN_POINT('Ctrl Pts',(3.5,36.7468000776565,-0.0564772772053694));
#5625=CARTESIAN_POINT('Ctrl Pts',(3.51835057975363,36.8718000776565,1.0807416596098));
#5626=CARTESIAN_POINT('Ctrl Pts',(2.86475599094327,36.9968000776565,2.01155730596849));
#5627=CARTESIAN_POINT('Ctrl Pts',(2.2111614021329,37.1218000776565,2.94237295232717));
#5628=CARTESIAN_POINT('Ctrl Pts',(1.13527256282109,37.2468000776565,3.31124536858055));
#5629=CARTESIAN_POINT('Ctrl Pts',(0.0593837235092791,37.3718000776565,3.68011778483394));
#5630=CARTESIAN_POINT('Ctrl Pts',(-1.02784639780354,37.4968000776565,3.34615024548552));
#5631=CARTESIAN_POINT('Ctrl Pts',(-2.11507651911636,37.6218000776565,3.01218270613711));
#5632=CARTESIAN_POINT('Ctrl Pts',(-2.79836296968137,37.7468000776565,2.10293946007882));
#5633=CARTESIAN_POINT('Ctrl Pts',(-3.48164942024637,37.8718000776565,1.19369621402054));
#5634=CARTESIAN_POINT('Ctrl Pts',(-3.5,37.9968000776565,0.0564772772053689));
#5635=CARTESIAN_POINT('Ctrl Pts',(-3.51835057975363,38.1218000776565,-1.0807416596098));
#5636=CARTESIAN_POINT('Ctrl Pts',(-2.86475599094327,38.2468000776565,-2.01155730596849));
#5637=CARTESIAN_POINT('Ctrl Pts',(-2.2111614021329,38.3718000776565,-2.94237295232717));
#5638=CARTESIAN_POINT('Ctrl Pts',(-1.13527256282109,38.4968000776565,-3.31124536858055));
#5639=CARTESIAN_POINT('Ctrl Pts',(-0.0593837235092786,38.6218000776565,
-3.68011778483394));
#5640=CARTESIAN_POINT('Ctrl Pts',(1.02784639780354,38.7468000776565,-3.34615024548552));
#5641=CARTESIAN_POINT('Ctrl Pts',(2.11507651911636,38.8718000776565,-3.01218270613711));
#5642=CARTESIAN_POINT('Ctrl Pts',(2.79836296968137,38.9968000776565,-2.10293946007882));
#5643=CARTESIAN_POINT('Ctrl Pts',(3.48164942024637,39.1218000776565,-1.19369621402054));
#5644=CARTESIAN_POINT('Ctrl Pts',(3.5,39.2468000776565,-0.0564772772053694));
#5645=CARTESIAN_POINT('Ctrl Pts',(3.51835057975363,39.3718000776565,1.0807416596098));
#5646=CARTESIAN_POINT('Ctrl Pts',(2.86475599094327,39.4968000776565,2.01155730596849));
#5647=CARTESIAN_POINT('Ctrl Pts',(2.2111614021329,39.6218000776565,2.94237295232717));
#5648=CARTESIAN_POINT('Ctrl Pts',(1.13527256282109,39.7468000776565,3.31124536858055));
#5649=CARTESIAN_POINT('Ctrl Pts',(0.0593837235092791,39.8718000776565,3.68011778483394));
#5650=CARTESIAN_POINT('Ctrl Pts',(-1.02784639780354,39.9968000776565,3.34615024548552));
#5651=CARTESIAN_POINT('Ctrl Pts',(-2.11507651911636,40.1218000776565,3.01218270613711));
#5652=CARTESIAN_POINT('Ctrl Pts',(-2.79836296968137,40.2468000776565,2.10293946007882));
#5653=CARTESIAN_POINT('Ctrl Pts',(-3.48164942024637,40.3718000776565,1.19369621402054));
#5654=CARTESIAN_POINT('Ctrl Pts',(-3.5,40.4968000776565,0.0564772772053685));
#5655=CARTESIAN_POINT('Origin',(-3.5,15.,3.664603343001E-14));
#5656=CARTESIAN_POINT('Origin',(-3.5,14.5031999223435,-0.0564772772052956));
#5657=CARTESIAN_POINT('',(-4.,15.,4.08336756143419E-14));
#5658=CARTESIAN_POINT('',(-3.5,15.,3.5649922684039E-14));
#5659=CARTESIAN_POINT('Origin',(-3.5,15.,3.664603343001E-14));
#5660=CARTESIAN_POINT('Origin',(-3.5,39.5031999223435,-0.0564772772052956));
#5661=CARTESIAN_POINT('Origin',(-3.5,40.,3.664603343001E-14));
#5662=CARTESIAN_POINT('Ctrl Pts',(-3.5,15.4968000776565,0.0564772772053689));
#5663=CARTESIAN_POINT('Ctrl Pts',(-3.51835057975363,15.6218000776565,-1.0807416596098));
#5664=CARTESIAN_POINT('Ctrl Pts',(-2.86475599094327,15.7468000776565,-2.01155730596849));
#5665=CARTESIAN_POINT('Ctrl Pts',(-2.2111614021329,15.8718000776565,-2.94237295232717));
#5666=CARTESIAN_POINT('Ctrl Pts',(-1.13527256282109,15.9968000776565,-3.31124536858055));
#5667=CARTESIAN_POINT('Ctrl Pts',(-0.0593837235092786,16.1218000776565,
-3.68011778483394));
#5668=CARTESIAN_POINT('Ctrl Pts',(1.02784639780354,16.2468000776565,-3.34615024548552));
#5669=CARTESIAN_POINT('Ctrl Pts',(2.11507651911636,16.3718000776565,-3.01218270613711));
#5670=CARTESIAN_POINT('Ctrl Pts',(2.79836296968137,16.4968000776565,-2.10293946007882));
#5671=CARTESIAN_POINT('Ctrl Pts',(3.48164942024637,16.6218000776565,-1.19369621402054));
#5672=CARTESIAN_POINT('Ctrl Pts',(3.5,16.7468000776565,-0.0564772772053694));
#5673=CARTESIAN_POINT('Ctrl Pts',(3.51835057975363,16.8718000776565,1.0807416596098));
#5674=CARTESIAN_POINT('Ctrl Pts',(2.86475599094327,16.9968000776565,2.01155730596849));
#5675=CARTESIAN_POINT('Ctrl Pts',(2.2111614021329,17.1218000776565,2.94237295232717));
#5676=CARTESIAN_POINT('Ctrl Pts',(1.13527256282109,17.2468000776565,3.31124536858055));
#5677=CARTESIAN_POINT('Ctrl Pts',(0.0593837235092791,17.3718000776565,3.68011778483394));
#5678=CARTESIAN_POINT('Ctrl Pts',(-1.02784639780354,17.4968000776565,3.34615024548552));
#5679=CARTESIAN_POINT('Ctrl Pts',(-2.11507651911636,17.6218000776565,3.01218270613711));
#5680=CARTESIAN_POINT('Ctrl Pts',(-2.79836296968137,17.7468000776565,2.10293946007882));
#5681=CARTESIAN_POINT('Ctrl Pts',(-3.48164942024637,17.8718000776565,1.19369621402054));
#5682=CARTESIAN_POINT('Ctrl Pts',(-3.5,17.9968000776565,0.0564772772053689));
#5683=CARTESIAN_POINT('Ctrl Pts',(-3.51835057975363,18.1218000776565,-1.0807416596098));
#5684=CARTESIAN_POINT('Ctrl Pts',(-2.86475599094327,18.2468000776565,-2.01155730596849));
#5685=CARTESIAN_POINT('Ctrl Pts',(-2.2111614021329,18.3718000776565,-2.94237295232717));
#5686=CARTESIAN_POINT('Ctrl Pts',(-1.13527256282109,18.4968000776565,-3.31124536858055));
#5687=CARTESIAN_POINT('Ctrl Pts',(-0.0593837235092786,18.6218000776565,
-3.68011778483394));
#5688=CARTESIAN_POINT('Ctrl Pts',(1.02784639780354,18.7468000776565,-3.34615024548552));
#5689=CARTESIAN_POINT('Ctrl Pts',(2.11507651911636,18.8718000776565,-3.01218270613711));
#5690=CARTESIAN_POINT('Ctrl Pts',(2.79836296968137,18.9968000776565,-2.10293946007882));
#5691=CARTESIAN_POINT('Ctrl Pts',(3.48164942024637,19.1218000776565,-1.19369621402054));
#5692=CARTESIAN_POINT('Ctrl Pts',(3.5,19.2468000776565,-0.0564772772053694));
#5693=CARTESIAN_POINT('Ctrl Pts',(3.51835057975363,19.3718000776565,1.0807416596098));
#5694=CARTESIAN_POINT('Ctrl Pts',(2.86475599094327,19.4968000776565,2.01155730596849));
#5695=CARTESIAN_POINT('Ctrl Pts',(2.2111614021329,19.6218000776565,2.94237295232717));
#5696=CARTESIAN_POINT('Ctrl Pts',(1.13527256282109,19.7468000776565,3.31124536858055));
#5697=CARTESIAN_POINT('Ctrl Pts',(0.0593837235092791,19.8718000776565,3.68011778483394));
#5698=CARTESIAN_POINT('Ctrl Pts',(-1.02784639780354,19.9968000776565,3.34615024548552));
#5699=CARTESIAN_POINT('Ctrl Pts',(-2.11507651911636,20.1218000776565,3.01218270613711));
#5700=CARTESIAN_POINT('Ctrl Pts',(-2.79836296968137,20.2468000776565,2.10293946007882));
#5701=CARTESIAN_POINT('Ctrl Pts',(-3.48164942024637,20.3718000776565,1.19369621402054));
#5702=CARTESIAN_POINT('Ctrl Pts',(-3.5,20.4968000776565,0.0564772772053689));
#5703=CARTESIAN_POINT('Ctrl Pts',(-3.51835057975363,20.6218000776565,-1.0807416596098));
#5704=CARTESIAN_POINT('Ctrl Pts',(-2.86475599094327,20.7468000776565,-2.01155730596849));
#5705=CARTESIAN_POINT('Ctrl Pts',(-2.2111614021329,20.8718000776565,-2.94237295232717));
#5706=CARTESIAN_POINT('Ctrl Pts',(-1.13527256282109,20.9968000776565,-3.31124536858055));
#5707=CARTESIAN_POINT('Ctrl Pts',(-0.0593837235092786,21.1218000776565,
-3.68011778483394));
#5708=CARTESIAN_POINT('Ctrl Pts',(1.02784639780354,21.2468000776565,-3.34615024548552));
#5709=CARTESIAN_POINT('Ctrl Pts',(2.11507651911636,21.3718000776565,-3.01218270613711));
#5710=CARTESIAN_POINT('Ctrl Pts',(2.79836296968137,21.4968000776565,-2.10293946007882));
#5711=CARTESIAN_POINT('Ctrl Pts',(3.48164942024637,21.6218000776565,-1.19369621402054));
#5712=CARTESIAN_POINT('Ctrl Pts',(3.5,21.7468000776565,-0.0564772772053694));
#5713=CARTESIAN_POINT('Ctrl Pts',(3.51835057975363,21.8718000776565,1.0807416596098));
#5714=CARTESIAN_POINT('Ctrl Pts',(2.86475599094327,21.9968000776565,2.01155730596849));
#5715=CARTESIAN_POINT('Ctrl Pts',(2.2111614021329,22.1218000776565,2.94237295232717));
#5716=CARTESIAN_POINT('Ctrl Pts',(1.13527256282109,22.2468000776565,3.31124536858055));
#5717=CARTESIAN_POINT('Ctrl Pts',(0.0593837235092791,22.3718000776565,3.68011778483394));
#5718=CARTESIAN_POINT('Ctrl Pts',(-1.02784639780354,22.4968000776565,3.34615024548552));
#5719=CARTESIAN_POINT('Ctrl Pts',(-2.11507651911636,22.6218000776565,3.01218270613711));
#5720=CARTESIAN_POINT('Ctrl Pts',(-2.79836296968137,22.7468000776565,2.10293946007882));
#5721=CARTESIAN_POINT('Ctrl Pts',(-3.48164942024637,22.8718000776565,1.19369621402054));
#5722=CARTESIAN_POINT('Ctrl Pts',(-3.5,22.9968000776565,0.0564772772053689));
#5723=CARTESIAN_POINT('Ctrl Pts',(-3.51835057975363,23.1218000776565,-1.0807416596098));
#5724=CARTESIAN_POINT('Ctrl Pts',(-2.86475599094327,23.2468000776565,-2.01155730596849));
#5725=CARTESIAN_POINT('Ctrl Pts',(-2.2111614021329,23.3718000776565,-2.94237295232717));
#5726=CARTESIAN_POINT('Ctrl Pts',(-1.13527256282109,23.4968000776565,-3.31124536858055));
#5727=CARTESIAN_POINT('Ctrl Pts',(-0.0593837235092786,23.6218000776565,
-3.68011778483394));
#5728=CARTESIAN_POINT('Ctrl Pts',(1.02784639780354,23.7468000776565,-3.34615024548552));
#5729=CARTESIAN_POINT('Ctrl Pts',(2.11507651911636,23.8718000776565,-3.01218270613711));
#5730=CARTESIAN_POINT('Ctrl Pts',(2.79836296968137,23.9968000776565,-2.10293946007882));
#5731=CARTESIAN_POINT('Ctrl Pts',(3.48164942024637,24.1218000776565,-1.19369621402054));
#5732=CARTESIAN_POINT('Ctrl Pts',(3.5,24.2468000776565,-0.0564772772053694));
#5733=CARTESIAN_POINT('Ctrl Pts',(3.51835057975363,24.3718000776565,1.0807416596098));
#5734=CARTESIAN_POINT('Ctrl Pts',(2.86475599094327,24.4968000776565,2.01155730596849));
#5735=CARTESIAN_POINT('Ctrl Pts',(2.2111614021329,24.6218000776565,2.94237295232717));
#5736=CARTESIAN_POINT('Ctrl Pts',(1.13527256282109,24.7468000776565,3.31124536858055));
#5737=CARTESIAN_POINT('Ctrl Pts',(0.0593837235092791,24.8718000776565,3.68011778483394));
#5738=CARTESIAN_POINT('Ctrl Pts',(-1.02784639780354,24.9968000776565,3.34615024548552));
#5739=CARTESIAN_POINT('Ctrl Pts',(-2.11507651911636,25.1218000776565,3.01218270613711));
#5740=CARTESIAN_POINT('Ctrl Pts',(-2.79836296968137,25.2468000776565,2.10293946007882));
#5741=CARTESIAN_POINT('Ctrl Pts',(-3.48164942024637,25.3718000776565,1.19369621402054));
#5742=CARTESIAN_POINT('Ctrl Pts',(-3.5,25.4968000776565,0.0564772772053689));
#5743=CARTESIAN_POINT('Ctrl Pts',(-3.51835057975363,25.6218000776565,-1.0807416596098));
#5744=CARTESIAN_POINT('Ctrl Pts',(-2.86475599094327,25.7468000776565,-2.01155730596849));
#5745=CARTESIAN_POINT('Ctrl Pts',(-2.2111614021329,25.8718000776565,-2.94237295232717));
#5746=CARTESIAN_POINT('Ctrl Pts',(-1.13527256282109,25.9968000776565,-3.31124536858055));
#5747=CARTESIAN_POINT('Ctrl Pts',(-0.0593837235092786,26.1218000776565,
-3.68011778483394));
#5748=CARTESIAN_POINT('Ctrl Pts',(1.02784639780354,26.2468000776565,-3.34615024548552));
#5749=CARTESIAN_POINT('Ctrl Pts',(2.11507651911636,26.3718000776565,-3.01218270613711));
#5750=CARTESIAN_POINT('Ctrl Pts',(2.79836296968137,26.4968000776565,-2.10293946007882));
#5751=CARTESIAN_POINT('Ctrl Pts',(3.48164942024637,26.6218000776565,-1.19369621402054));
#5752=CARTESIAN_POINT('Ctrl Pts',(3.5,26.7468000776565,-0.0564772772053694));
#5753=CARTESIAN_POINT('Ctrl Pts',(3.51835057975363,26.8718000776565,1.0807416596098));
#5754=CARTESIAN_POINT('Ctrl Pts',(2.86475599094327,26.9968000776565,2.01155730596849));
#5755=CARTESIAN_POINT('Ctrl Pts',(2.2111614021329,27.1218000776565,2.94237295232717));
#5756=CARTESIAN_POINT('Ctrl Pts',(1.13527256282109,27.2468000776565,3.31124536858055));
#5757=CARTESIAN_POINT('Ctrl Pts',(0.0593837235092791,27.3718000776565,3.68011778483394));
#5758=CARTESIAN_POINT('Ctrl Pts',(-1.02784639780354,27.4968000776565,3.34615024548552));
#5759=CARTESIAN_POINT('Ctrl Pts',(-2.11507651911636,27.6218000776565,3.01218270613711));
#5760=CARTESIAN_POINT('Ctrl Pts',(-2.79836296968137,27.7468000776565,2.10293946007882));
#5761=CARTESIAN_POINT('Ctrl Pts',(-3.48164942024637,27.8718000776565,1.19369621402054));
#5762=CARTESIAN_POINT('Ctrl Pts',(-3.5,27.9968000776565,0.0564772772053689));
#5763=CARTESIAN_POINT('Ctrl Pts',(-3.51835057975363,28.1218000776565,-1.0807416596098));
#5764=CARTESIAN_POINT('Ctrl Pts',(-2.86475599094327,28.2468000776565,-2.01155730596849));
#5765=CARTESIAN_POINT('Ctrl Pts',(-2.2111614021329,28.3718000776565,-2.94237295232717));
#5766=CARTESIAN_POINT('Ctrl Pts',(-1.13527256282109,28.4968000776565,-3.31124536858055));
#5767=CARTESIAN_POINT('Ctrl Pts',(-0.0593837235092786,28.6218000776565,
-3.68011778483394));
#5768=CARTESIAN_POINT('Ctrl Pts',(1.02784639780354,28.7468000776565,-3.34615024548552));
#5769=CARTESIAN_POINT('Ctrl Pts',(2.11507651911636,28.8718000776565,-3.01218270613711));
#5770=CARTESIAN_POINT('Ctrl Pts',(2.79836296968137,28.9968000776565,-2.10293946007882));
#5771=CARTESIAN_POINT('Ctrl Pts',(3.48164942024637,29.1218000776565,-1.19369621402054));
#5772=CARTESIAN_POINT('Ctrl Pts',(3.5,29.2468000776565,-0.0564772772053694));
#5773=CARTESIAN_POINT('Ctrl Pts',(3.51835057975363,29.3718000776565,1.0807416596098));
#5774=CARTESIAN_POINT('Ctrl Pts',(2.86475599094327,29.4968000776565,2.01155730596849));
#5775=CARTESIAN_POINT('Ctrl Pts',(2.2111614021329,29.6218000776565,2.94237295232717));
#5776=CARTESIAN_POINT('Ctrl Pts',(1.13527256282109,29.7468000776565,3.31124536858055));
#5777=CARTESIAN_POINT('Ctrl Pts',(0.0593837235092791,29.8718000776565,3.68011778483394));
#5778=CARTESIAN_POINT('Ctrl Pts',(-1.02784639780354,29.9968000776565,3.34615024548552));
#5779=CARTESIAN_POINT('Ctrl Pts',(-2.11507651911636,30.1218000776565,3.01218270613711));
#5780=CARTESIAN_POINT('Ctrl Pts',(-2.79836296968137,30.2468000776565,2.10293946007882));
#5781=CARTESIAN_POINT('Ctrl Pts',(-3.48164942024637,30.3718000776565,1.19369621402054));
#5782=CARTESIAN_POINT('Ctrl Pts',(-3.5,30.4968000776565,0.0564772772053689));
#5783=CARTESIAN_POINT('Ctrl Pts',(-3.51835057975363,30.6218000776565,-1.0807416596098));
#5784=CARTESIAN_POINT('Ctrl Pts',(-2.86475599094327,30.7468000776565,-2.01155730596849));
#5785=CARTESIAN_POINT('Ctrl Pts',(-2.2111614021329,30.8718000776565,-2.94237295232717));
#5786=CARTESIAN_POINT('Ctrl Pts',(-1.13527256282109,30.9968000776565,-3.31124536858055));
#5787=CARTESIAN_POINT('Ctrl Pts',(-0.0593837235092786,31.1218000776565,
-3.68011778483394));
#5788=CARTESIAN_POINT('Ctrl Pts',(1.02784639780354,31.2468000776565,-3.34615024548552));
#5789=CARTESIAN_POINT('Ctrl Pts',(2.11507651911636,31.3718000776565,-3.01218270613711));
#5790=CARTESIAN_POINT('Ctrl Pts',(2.79836296968137,31.4968000776565,-2.10293946007882));
#5791=CARTESIAN_POINT('Ctrl Pts',(3.48164942024637,31.6218000776565,-1.19369621402054));
#5792=CARTESIAN_POINT('Ctrl Pts',(3.5,31.7468000776565,-0.0564772772053694));
#5793=CARTESIAN_POINT('Ctrl Pts',(3.51835057975363,31.8718000776565,1.0807416596098));
#5794=CARTESIAN_POINT('Ctrl Pts',(2.86475599094327,31.9968000776565,2.01155730596849));
#5795=CARTESIAN_POINT('Ctrl Pts',(2.2111614021329,32.1218000776565,2.94237295232717));
#5796=CARTESIAN_POINT('Ctrl Pts',(1.13527256282109,32.2468000776565,3.31124536858055));
#5797=CARTESIAN_POINT('Ctrl Pts',(0.0593837235092791,32.3718000776565,3.68011778483394));
#5798=CARTESIAN_POINT('Ctrl Pts',(-1.02784639780354,32.4968000776565,3.34615024548552));
#5799=CARTESIAN_POINT('Ctrl Pts',(-2.11507651911636,32.6218000776565,3.01218270613711));
#5800=CARTESIAN_POINT('Ctrl Pts',(-2.79836296968137,32.7468000776565,2.10293946007882));
#5801=CARTESIAN_POINT('Ctrl Pts',(-3.48164942024637,32.8718000776565,1.19369621402054));
#5802=CARTESIAN_POINT('Ctrl Pts',(-3.5,32.9968000776565,0.0564772772053689));
#5803=CARTESIAN_POINT('Ctrl Pts',(-3.51835057975363,33.1218000776565,-1.0807416596098));
#5804=CARTESIAN_POINT('Ctrl Pts',(-2.86475599094327,33.2468000776565,-2.01155730596849));
#5805=CARTESIAN_POINT('Ctrl Pts',(-2.2111614021329,33.3718000776565,-2.94237295232717));
#5806=CARTESIAN_POINT('Ctrl Pts',(-1.13527256282109,33.4968000776565,-3.31124536858055));
#5807=CARTESIAN_POINT('Ctrl Pts',(-0.0593837235092786,33.6218000776565,
-3.68011778483394));
#5808=CARTESIAN_POINT('Ctrl Pts',(1.02784639780354,33.7468000776565,-3.34615024548552));
#5809=CARTESIAN_POINT('Ctrl Pts',(2.11507651911636,33.8718000776565,-3.01218270613711));
#5810=CARTESIAN_POINT('Ctrl Pts',(2.79836296968137,33.9968000776565,-2.10293946007882));
#5811=CARTESIAN_POINT('Ctrl Pts',(3.48164942024637,34.1218000776565,-1.19369621402054));
#5812=CARTESIAN_POINT('Ctrl Pts',(3.5,34.2468000776565,-0.0564772772053694));
#5813=CARTESIAN_POINT('Ctrl Pts',(3.51835057975363,34.3718000776565,1.0807416596098));
#5814=CARTESIAN_POINT('Ctrl Pts',(2.86475599094327,34.4968000776565,2.01155730596849));
#5815=CARTESIAN_POINT('Ctrl Pts',(2.2111614021329,34.6218000776565,2.94237295232717));
#5816=CARTESIAN_POINT('Ctrl Pts',(1.13527256282109,34.7468000776565,3.31124536858055));
#5817=CARTESIAN_POINT('Ctrl Pts',(0.0593837235092791,34.8718000776565,3.68011778483394));
#5818=CARTESIAN_POINT('Ctrl Pts',(-1.02784639780354,34.9968000776565,3.34615024548552));
#5819=CARTESIAN_POINT('Ctrl Pts',(-2.11507651911636,35.1218000776565,3.01218270613711));
#5820=CARTESIAN_POINT('Ctrl Pts',(-2.79836296968137,35.2468000776565,2.10293946007882));
#5821=CARTESIAN_POINT('Ctrl Pts',(-3.48164942024637,35.3718000776565,1.19369621402054));
#5822=CARTESIAN_POINT('Ctrl Pts',(-3.5,35.4968000776565,0.0564772772053689));
#5823=CARTESIAN_POINT('Ctrl Pts',(-3.51835057975363,35.6218000776565,-1.0807416596098));
#5824=CARTESIAN_POINT('Ctrl Pts',(-2.86475599094327,35.7468000776565,-2.01155730596849));
#5825=CARTESIAN_POINT('Ctrl Pts',(-2.2111614021329,35.8718000776565,-2.94237295232717));
#5826=CARTESIAN_POINT('Ctrl Pts',(-1.13527256282109,35.9968000776565,-3.31124536858055));
#5827=CARTESIAN_POINT('Ctrl Pts',(-0.0593837235092786,36.1218000776565,
-3.68011778483394));
#5828=CARTESIAN_POINT('Ctrl Pts',(1.02784639780354,36.2468000776565,-3.34615024548552));
#5829=CARTESIAN_POINT('Ctrl Pts',(2.11507651911636,36.3718000776565,-3.01218270613711));
#5830=CARTESIAN_POINT('Ctrl Pts',(2.79836296968137,36.4968000776565,-2.10293946007882));
#5831=CARTESIAN_POINT('Ctrl Pts',(3.48164942024637,36.6218000776565,-1.19369621402054));
#5832=CARTESIAN_POINT('Ctrl Pts',(3.5,36.7468000776565,-0.0564772772053694));
#5833=CARTESIAN_POINT('Ctrl Pts',(3.51835057975363,36.8718000776565,1.0807416596098));
#5834=CARTESIAN_POINT('Ctrl Pts',(2.86475599094327,36.9968000776565,2.01155730596849));
#5835=CARTESIAN_POINT('Ctrl Pts',(2.2111614021329,37.1218000776565,2.94237295232717));
#5836=CARTESIAN_POINT('Ctrl Pts',(1.13527256282109,37.2468000776565,3.31124536858055));
#5837=CARTESIAN_POINT('Ctrl Pts',(0.0593837235092791,37.3718000776565,3.68011778483394));
#5838=CARTESIAN_POINT('Ctrl Pts',(-1.02784639780354,37.4968000776565,3.34615024548552));
#5839=CARTESIAN_POINT('Ctrl Pts',(-2.11507651911636,37.6218000776565,3.01218270613711));
#5840=CARTESIAN_POINT('Ctrl Pts',(-2.79836296968137,37.7468000776565,2.10293946007882));
#5841=CARTESIAN_POINT('Ctrl Pts',(-3.48164942024637,37.8718000776565,1.19369621402054));
#5842=CARTESIAN_POINT('Ctrl Pts',(-3.5,37.9968000776565,0.0564772772053689));
#5843=CARTESIAN_POINT('Ctrl Pts',(-3.51835057975363,38.1218000776565,-1.0807416596098));
#5844=CARTESIAN_POINT('Ctrl Pts',(-2.86475599094327,38.2468000776565,-2.01155730596849));
#5845=CARTESIAN_POINT('Ctrl Pts',(-2.2111614021329,38.3718000776565,-2.94237295232717));
#5846=CARTESIAN_POINT('Ctrl Pts',(-1.13527256282109,38.4968000776565,-3.31124536858055));
#5847=CARTESIAN_POINT('Ctrl Pts',(-0.0593837235092786,38.6218000776565,
-3.68011778483394));
#5848=CARTESIAN_POINT('Ctrl Pts',(1.02784639780354,38.7468000776565,-3.34615024548552));
#5849=CARTESIAN_POINT('Ctrl Pts',(2.11507651911636,38.8718000776565,-3.01218270613711));
#5850=CARTESIAN_POINT('Ctrl Pts',(2.79836296968137,38.9968000776565,-2.10293946007882));
#5851=CARTESIAN_POINT('Ctrl Pts',(3.48164942024637,39.1218000776565,-1.19369621402054));
#5852=CARTESIAN_POINT('Ctrl Pts',(3.5,39.2468000776565,-0.0564772772053694));
#5853=CARTESIAN_POINT('Ctrl Pts',(3.51835057975363,39.3718000776565,1.0807416596098));
#5854=CARTESIAN_POINT('Ctrl Pts',(2.86475599094327,39.4968000776565,2.01155730596849));
#5855=CARTESIAN_POINT('Ctrl Pts',(2.2111614021329,39.6218000776565,2.94237295232717));
#5856=CARTESIAN_POINT('Ctrl Pts',(1.13527256282109,39.7468000776565,3.31124536858055));
#5857=CARTESIAN_POINT('Ctrl Pts',(0.0593837235092791,39.8718000776565,3.68011778483394));
#5858=CARTESIAN_POINT('Ctrl Pts',(-1.02784639780354,39.9968000776565,3.34615024548552));
#5859=CARTESIAN_POINT('Ctrl Pts',(-2.11507651911636,40.1218000776565,3.01218270613711));
#5860=CARTESIAN_POINT('Ctrl Pts',(-2.79836296968137,40.2468000776565,2.10293946007882));
#5861=CARTESIAN_POINT('Ctrl Pts',(-3.48164942024637,40.3718000776565,1.19369621402054));
#5862=CARTESIAN_POINT('Ctrl Pts',(-3.5,40.4968000776565,0.0564772772053689));
#5863=CARTESIAN_POINT('Ctrl Pts',(-2.5,15.4968000776565,0.0564772772053586));
#5864=CARTESIAN_POINT('Ctrl Pts',(-2.51835057975363,15.6218000776565,-0.755821963376908));
#5865=CARTESIAN_POINT('Ctrl Pts',(-2.05573899656831,15.7468000776565,-1.42377205367602));
#5866=CARTESIAN_POINT('Ctrl Pts',(-1.593127413383,15.8718000776565,-2.09172214397514));
#5867=CARTESIAN_POINT('Ctrl Pts',(-0.826255568446133,15.9968000776565,-2.3601888522854));
#5868=CARTESIAN_POINT('Ctrl Pts',(-0.0593837235092677,16.1218000776565,
-2.62865556059567));
#5869=CARTESIAN_POINT('Ctrl Pts',(0.718829403428605,16.2468000776565,-2.39509372919037));
#5870=CARTESIAN_POINT('Ctrl Pts',(1.49704253036648,16.3718000776565,-2.16153189778506));
#5871=CARTESIAN_POINT('Ctrl Pts',(1.98934597530643,16.4968000776565,-1.51515420778634));
#5872=CARTESIAN_POINT('Ctrl Pts',(2.48164942024637,16.6218000776565,-0.868776517787625));
#5873=CARTESIAN_POINT('Ctrl Pts',(2.5,16.7468000776565,-0.0564772772053589));
#5874=CARTESIAN_POINT('Ctrl Pts',(2.51835057975363,16.8718000776565,0.755821963376907));
#5875=CARTESIAN_POINT('Ctrl Pts',(2.05573899656831,16.9968000776565,1.42377205367602));
#5876=CARTESIAN_POINT('Ctrl Pts',(1.593127413383,17.1218000776565,2.09172214397514));
#5877=CARTESIAN_POINT('Ctrl Pts',(0.826255568446133,17.2468000776565,2.3601888522854));
#5878=CARTESIAN_POINT('Ctrl Pts',(0.059383723509268,17.3718000776565,2.62865556059567));
#5879=CARTESIAN_POINT('Ctrl Pts',(-0.718829403428604,17.4968000776565,2.39509372919037));
#5880=CARTESIAN_POINT('Ctrl Pts',(-1.49704253036648,17.6218000776565,2.16153189778506));
#5881=CARTESIAN_POINT('Ctrl Pts',(-1.98934597530643,17.7468000776565,1.51515420778634));
#5882=CARTESIAN_POINT('Ctrl Pts',(-2.48164942024637,17.8718000776565,0.868776517787626));
#5883=CARTESIAN_POINT('Ctrl Pts',(-2.5,17.9968000776565,0.0564772772053586));
#5884=CARTESIAN_POINT('Ctrl Pts',(-2.51835057975363,18.1218000776565,-0.755821963376908));
#5885=CARTESIAN_POINT('Ctrl Pts',(-2.05573899656831,18.2468000776565,-1.42377205367602));
#5886=CARTESIAN_POINT('Ctrl Pts',(-1.593127413383,18.3718000776565,-2.09172214397514));
#5887=CARTESIAN_POINT('Ctrl Pts',(-0.826255568446133,18.4968000776565,-2.3601888522854));
#5888=CARTESIAN_POINT('Ctrl Pts',(-0.0593837235092677,18.6218000776565,
-2.62865556059567));
#5889=CARTESIAN_POINT('Ctrl Pts',(0.718829403428605,18.7468000776565,-2.39509372919037));
#5890=CARTESIAN_POINT('Ctrl Pts',(1.49704253036648,18.8718000776565,-2.16153189778506));
#5891=CARTESIAN_POINT('Ctrl Pts',(1.98934597530643,18.9968000776565,-1.51515420778634));
#5892=CARTESIAN_POINT('Ctrl Pts',(2.48164942024637,19.1218000776565,-0.868776517787625));
#5893=CARTESIAN_POINT('Ctrl Pts',(2.5,19.2468000776565,-0.0564772772053589));
#5894=CARTESIAN_POINT('Ctrl Pts',(2.51835057975363,19.3718000776565,0.755821963376907));
#5895=CARTESIAN_POINT('Ctrl Pts',(2.05573899656831,19.4968000776565,1.42377205367602));
#5896=CARTESIAN_POINT('Ctrl Pts',(1.593127413383,19.6218000776565,2.09172214397514));
#5897=CARTESIAN_POINT('Ctrl Pts',(0.826255568446133,19.7468000776565,2.3601888522854));
#5898=CARTESIAN_POINT('Ctrl Pts',(0.059383723509268,19.8718000776565,2.62865556059567));
#5899=CARTESIAN_POINT('Ctrl Pts',(-0.718829403428604,19.9968000776565,2.39509372919037));
#5900=CARTESIAN_POINT('Ctrl Pts',(-1.49704253036648,20.1218000776565,2.16153189778506));
#5901=CARTESIAN_POINT('Ctrl Pts',(-1.98934597530643,20.2468000776565,1.51515420778634));
#5902=CARTESIAN_POINT('Ctrl Pts',(-2.48164942024637,20.3718000776565,0.868776517787626));
#5903=CARTESIAN_POINT('Ctrl Pts',(-2.5,20.4968000776565,0.0564772772053586));
#5904=CARTESIAN_POINT('Ctrl Pts',(-2.51835057975363,20.6218000776565,-0.755821963376908));
#5905=CARTESIAN_POINT('Ctrl Pts',(-2.05573899656831,20.7468000776565,-1.42377205367602));
#5906=CARTESIAN_POINT('Ctrl Pts',(-1.593127413383,20.8718000776565,-2.09172214397514));
#5907=CARTESIAN_POINT('Ctrl Pts',(-0.826255568446133,20.9968000776565,-2.3601888522854));
#5908=CARTESIAN_POINT('Ctrl Pts',(-0.0593837235092677,21.1218000776565,
-2.62865556059567));
#5909=CARTESIAN_POINT('Ctrl Pts',(0.718829403428605,21.2468000776565,-2.39509372919037));
#5910=CARTESIAN_POINT('Ctrl Pts',(1.49704253036648,21.3718000776565,-2.16153189778506));
#5911=CARTESIAN_POINT('Ctrl Pts',(1.98934597530643,21.4968000776565,-1.51515420778634));
#5912=CARTESIAN_POINT('Ctrl Pts',(2.48164942024637,21.6218000776565,-0.868776517787625));
#5913=CARTESIAN_POINT('Ctrl Pts',(2.5,21.7468000776565,-0.0564772772053589));
#5914=CARTESIAN_POINT('Ctrl Pts',(2.51835057975363,21.8718000776565,0.755821963376907));
#5915=CARTESIAN_POINT('Ctrl Pts',(2.05573899656831,21.9968000776565,1.42377205367602));
#5916=CARTESIAN_POINT('Ctrl Pts',(1.593127413383,22.1218000776565,2.09172214397514));
#5917=CARTESIAN_POINT('Ctrl Pts',(0.826255568446133,22.2468000776565,2.3601888522854));
#5918=CARTESIAN_POINT('Ctrl Pts',(0.059383723509268,22.3718000776565,2.62865556059567));
#5919=CARTESIAN_POINT('Ctrl Pts',(-0.718829403428604,22.4968000776565,2.39509372919037));
#5920=CARTESIAN_POINT('Ctrl Pts',(-1.49704253036648,22.6218000776565,2.16153189778506));
#5921=CARTESIAN_POINT('Ctrl Pts',(-1.98934597530643,22.7468000776565,1.51515420778634));
#5922=CARTESIAN_POINT('Ctrl Pts',(-2.48164942024637,22.8718000776565,0.868776517787626));
#5923=CARTESIAN_POINT('Ctrl Pts',(-2.5,22.9968000776565,0.0564772772053586));
#5924=CARTESIAN_POINT('Ctrl Pts',(-2.51835057975363,23.1218000776565,-0.755821963376908));
#5925=CARTESIAN_POINT('Ctrl Pts',(-2.05573899656831,23.2468000776565,-1.42377205367602));
#5926=CARTESIAN_POINT('Ctrl Pts',(-1.593127413383,23.3718000776565,-2.09172214397514));
#5927=CARTESIAN_POINT('Ctrl Pts',(-0.826255568446133,23.4968000776565,-2.3601888522854));
#5928=CARTESIAN_POINT('Ctrl Pts',(-0.0593837235092677,23.6218000776565,
-2.62865556059567));
#5929=CARTESIAN_POINT('Ctrl Pts',(0.718829403428605,23.7468000776565,-2.39509372919037));
#5930=CARTESIAN_POINT('Ctrl Pts',(1.49704253036648,23.8718000776565,-2.16153189778506));
#5931=CARTESIAN_POINT('Ctrl Pts',(1.98934597530643,23.9968000776565,-1.51515420778634));
#5932=CARTESIAN_POINT('Ctrl Pts',(2.48164942024637,24.1218000776565,-0.868776517787625));
#5933=CARTESIAN_POINT('Ctrl Pts',(2.5,24.2468000776565,-0.0564772772053589));
#5934=CARTESIAN_POINT('Ctrl Pts',(2.51835057975363,24.3718000776565,0.755821963376907));
#5935=CARTESIAN_POINT('Ctrl Pts',(2.05573899656831,24.4968000776565,1.42377205367602));
#5936=CARTESIAN_POINT('Ctrl Pts',(1.593127413383,24.6218000776565,2.09172214397514));
#5937=CARTESIAN_POINT('Ctrl Pts',(0.826255568446133,24.7468000776565,2.3601888522854));
#5938=CARTESIAN_POINT('Ctrl Pts',(0.059383723509268,24.8718000776565,2.62865556059567));
#5939=CARTESIAN_POINT('Ctrl Pts',(-0.718829403428604,24.9968000776565,2.39509372919037));
#5940=CARTESIAN_POINT('Ctrl Pts',(-1.49704253036648,25.1218000776565,2.16153189778506));
#5941=CARTESIAN_POINT('Ctrl Pts',(-1.98934597530643,25.2468000776565,1.51515420778634));
#5942=CARTESIAN_POINT('Ctrl Pts',(-2.48164942024637,25.3718000776565,0.868776517787626));
#5943=CARTESIAN_POINT('Ctrl Pts',(-2.5,25.4968000776565,0.0564772772053586));
#5944=CARTESIAN_POINT('Ctrl Pts',(-2.51835057975363,25.6218000776565,-0.755821963376908));
#5945=CARTESIAN_POINT('Ctrl Pts',(-2.05573899656831,25.7468000776565,-1.42377205367602));
#5946=CARTESIAN_POINT('Ctrl Pts',(-1.593127413383,25.8718000776565,-2.09172214397514));
#5947=CARTESIAN_POINT('Ctrl Pts',(-0.826255568446133,25.9968000776565,-2.3601888522854));
#5948=CARTESIAN_POINT('Ctrl Pts',(-0.0593837235092677,26.1218000776565,
-2.62865556059567));
#5949=CARTESIAN_POINT('Ctrl Pts',(0.718829403428605,26.2468000776565,-2.39509372919037));
#5950=CARTESIAN_POINT('Ctrl Pts',(1.49704253036648,26.3718000776565,-2.16153189778506));
#5951=CARTESIAN_POINT('Ctrl Pts',(1.98934597530643,26.4968000776565,-1.51515420778634));
#5952=CARTESIAN_POINT('Ctrl Pts',(2.48164942024637,26.6218000776565,-0.868776517787625));
#5953=CARTESIAN_POINT('Ctrl Pts',(2.5,26.7468000776565,-0.0564772772053589));
#5954=CARTESIAN_POINT('Ctrl Pts',(2.51835057975363,26.8718000776565,0.755821963376907));
#5955=CARTESIAN_POINT('Ctrl Pts',(2.05573899656831,26.9968000776565,1.42377205367602));
#5956=CARTESIAN_POINT('Ctrl Pts',(1.593127413383,27.1218000776565,2.09172214397514));
#5957=CARTESIAN_POINT('Ctrl Pts',(0.826255568446133,27.2468000776565,2.3601888522854));
#5958=CARTESIAN_POINT('Ctrl Pts',(0.059383723509268,27.3718000776565,2.62865556059567));
#5959=CARTESIAN_POINT('Ctrl Pts',(-0.718829403428604,27.4968000776565,2.39509372919037));
#5960=CARTESIAN_POINT('Ctrl Pts',(-1.49704253036648,27.6218000776565,2.16153189778506));
#5961=CARTESIAN_POINT('Ctrl Pts',(-1.98934597530643,27.7468000776565,1.51515420778634));
#5962=CARTESIAN_POINT('Ctrl Pts',(-2.48164942024637,27.8718000776565,0.868776517787626));
#5963=CARTESIAN_POINT('Ctrl Pts',(-2.5,27.9968000776565,0.0564772772053586));
#5964=CARTESIAN_POINT('Ctrl Pts',(-2.51835057975363,28.1218000776565,-0.755821963376908));
#5965=CARTESIAN_POINT('Ctrl Pts',(-2.05573899656831,28.2468000776565,-1.42377205367602));
#5966=CARTESIAN_POINT('Ctrl Pts',(-1.593127413383,28.3718000776565,-2.09172214397514));
#5967=CARTESIAN_POINT('Ctrl Pts',(-0.826255568446133,28.4968000776565,-2.3601888522854));
#5968=CARTESIAN_POINT('Ctrl Pts',(-0.0593837235092677,28.6218000776565,
-2.62865556059567));
#5969=CARTESIAN_POINT('Ctrl Pts',(0.718829403428605,28.7468000776565,-2.39509372919037));
#5970=CARTESIAN_POINT('Ctrl Pts',(1.49704253036648,28.8718000776565,-2.16153189778506));
#5971=CARTESIAN_POINT('Ctrl Pts',(1.98934597530643,28.9968000776565,-1.51515420778634));
#5972=CARTESIAN_POINT('Ctrl Pts',(2.48164942024637,29.1218000776565,-0.868776517787625));
#5973=CARTESIAN_POINT('Ctrl Pts',(2.5,29.2468000776565,-0.0564772772053589));
#5974=CARTESIAN_POINT('Ctrl Pts',(2.51835057975363,29.3718000776565,0.755821963376907));
#5975=CARTESIAN_POINT('Ctrl Pts',(2.05573899656831,29.4968000776565,1.42377205367602));
#5976=CARTESIAN_POINT('Ctrl Pts',(1.593127413383,29.6218000776565,2.09172214397514));
#5977=CARTESIAN_POINT('Ctrl Pts',(0.826255568446133,29.7468000776565,2.3601888522854));
#5978=CARTESIAN_POINT('Ctrl Pts',(0.059383723509268,29.8718000776565,2.62865556059567));
#5979=CARTESIAN_POINT('Ctrl Pts',(-0.718829403428604,29.9968000776565,2.39509372919037));
#5980=CARTESIAN_POINT('Ctrl Pts',(-1.49704253036648,30.1218000776565,2.16153189778506));
#5981=CARTESIAN_POINT('Ctrl Pts',(-1.98934597530643,30.2468000776565,1.51515420778634));
#5982=CARTESIAN_POINT('Ctrl Pts',(-2.48164942024637,30.3718000776565,0.868776517787626));
#5983=CARTESIAN_POINT('Ctrl Pts',(-2.5,30.4968000776565,0.0564772772053586));
#5984=CARTESIAN_POINT('Ctrl Pts',(-2.51835057975363,30.6218000776565,-0.755821963376908));
#5985=CARTESIAN_POINT('Ctrl Pts',(-2.05573899656831,30.7468000776565,-1.42377205367602));
#5986=CARTESIAN_POINT('Ctrl Pts',(-1.593127413383,30.8718000776565,-2.09172214397514));
#5987=CARTESIAN_POINT('Ctrl Pts',(-0.826255568446133,30.9968000776565,-2.3601888522854));
#5988=CARTESIAN_POINT('Ctrl Pts',(-0.0593837235092677,31.1218000776565,
-2.62865556059567));
#5989=CARTESIAN_POINT('Ctrl Pts',(0.718829403428605,31.2468000776565,-2.39509372919037));
#5990=CARTESIAN_POINT('Ctrl Pts',(1.49704253036648,31.3718000776565,-2.16153189778506));
#5991=CARTESIAN_POINT('Ctrl Pts',(1.98934597530643,31.4968000776565,-1.51515420778634));
#5992=CARTESIAN_POINT('Ctrl Pts',(2.48164942024637,31.6218000776565,-0.868776517787625));
#5993=CARTESIAN_POINT('Ctrl Pts',(2.5,31.7468000776565,-0.0564772772053589));
#5994=CARTESIAN_POINT('Ctrl Pts',(2.51835057975363,31.8718000776565,0.755821963376907));
#5995=CARTESIAN_POINT('Ctrl Pts',(2.05573899656831,31.9968000776565,1.42377205367602));
#5996=CARTESIAN_POINT('Ctrl Pts',(1.593127413383,32.1218000776565,2.09172214397514));
#5997=CARTESIAN_POINT('Ctrl Pts',(0.826255568446133,32.2468000776565,2.3601888522854));
#5998=CARTESIAN_POINT('Ctrl Pts',(0.059383723509268,32.3718000776565,2.62865556059567));
#5999=CARTESIAN_POINT('Ctrl Pts',(-0.718829403428604,32.4968000776565,2.39509372919037));
#6000=CARTESIAN_POINT('Ctrl Pts',(-1.49704253036648,32.6218000776565,2.16153189778506));
#6001=CARTESIAN_POINT('Ctrl Pts',(-1.98934597530643,32.7468000776565,1.51515420778634));
#6002=CARTESIAN_POINT('Ctrl Pts',(-2.48164942024637,32.8718000776565,0.868776517787626));
#6003=CARTESIAN_POINT('Ctrl Pts',(-2.5,32.9968000776565,0.0564772772053586));
#6004=CARTESIAN_POINT('Ctrl Pts',(-2.51835057975363,33.1218000776565,-0.755821963376908));
#6005=CARTESIAN_POINT('Ctrl Pts',(-2.05573899656831,33.2468000776565,-1.42377205367602));
#6006=CARTESIAN_POINT('Ctrl Pts',(-1.593127413383,33.3718000776565,-2.09172214397514));
#6007=CARTESIAN_POINT('Ctrl Pts',(-0.826255568446133,33.4968000776565,-2.3601888522854));
#6008=CARTESIAN_POINT('Ctrl Pts',(-0.0593837235092677,33.6218000776565,
-2.62865556059567));
#6009=CARTESIAN_POINT('Ctrl Pts',(0.718829403428605,33.7468000776565,-2.39509372919037));
#6010=CARTESIAN_POINT('Ctrl Pts',(1.49704253036648,33.8718000776565,-2.16153189778506));
#6011=CARTESIAN_POINT('Ctrl Pts',(1.98934597530643,33.9968000776565,-1.51515420778634));
#6012=CARTESIAN_POINT('Ctrl Pts',(2.48164942024637,34.1218000776565,-0.868776517787625));
#6013=CARTESIAN_POINT('Ctrl Pts',(2.5,34.2468000776565,-0.0564772772053589));
#6014=CARTESIAN_POINT('Ctrl Pts',(2.51835057975363,34.3718000776565,0.755821963376907));
#6015=CARTESIAN_POINT('Ctrl Pts',(2.05573899656831,34.4968000776565,1.42377205367602));
#6016=CARTESIAN_POINT('Ctrl Pts',(1.593127413383,34.6218000776565,2.09172214397514));
#6017=CARTESIAN_POINT('Ctrl Pts',(0.826255568446133,34.7468000776565,2.3601888522854));
#6018=CARTESIAN_POINT('Ctrl Pts',(0.059383723509268,34.8718000776565,2.62865556059567));
#6019=CARTESIAN_POINT('Ctrl Pts',(-0.718829403428604,34.9968000776565,2.39509372919037));
#6020=CARTESIAN_POINT('Ctrl Pts',(-1.49704253036648,35.1218000776565,2.16153189778506));
#6021=CARTESIAN_POINT('Ctrl Pts',(-1.98934597530643,35.2468000776565,1.51515420778634));
#6022=CARTESIAN_POINT('Ctrl Pts',(-2.48164942024637,35.3718000776565,0.868776517787626));
#6023=CARTESIAN_POINT('Ctrl Pts',(-2.5,35.4968000776565,0.0564772772053586));
#6024=CARTESIAN_POINT('Ctrl Pts',(-2.51835057975363,35.6218000776565,-0.755821963376908));
#6025=CARTESIAN_POINT('Ctrl Pts',(-2.05573899656831,35.7468000776565,-1.42377205367602));
#6026=CARTESIAN_POINT('Ctrl Pts',(-1.593127413383,35.8718000776565,-2.09172214397514));
#6027=CARTESIAN_POINT('Ctrl Pts',(-0.826255568446133,35.9968000776565,-2.3601888522854));
#6028=CARTESIAN_POINT('Ctrl Pts',(-0.0593837235092677,36.1218000776565,
-2.62865556059567));
#6029=CARTESIAN_POINT('Ctrl Pts',(0.718829403428605,36.2468000776565,-2.39509372919037));
#6030=CARTESIAN_POINT('Ctrl Pts',(1.49704253036648,36.3718000776565,-2.16153189778506));
#6031=CARTESIAN_POINT('Ctrl Pts',(1.98934597530643,36.4968000776565,-1.51515420778634));
#6032=CARTESIAN_POINT('Ctrl Pts',(2.48164942024637,36.6218000776565,-0.868776517787625));
#6033=CARTESIAN_POINT('Ctrl Pts',(2.5,36.7468000776565,-0.0564772772053589));
#6034=CARTESIAN_POINT('Ctrl Pts',(2.51835057975363,36.8718000776565,0.755821963376907));
#6035=CARTESIAN_POINT('Ctrl Pts',(2.05573899656831,36.9968000776565,1.42377205367602));
#6036=CARTESIAN_POINT('Ctrl Pts',(1.593127413383,37.1218000776565,2.09172214397514));
#6037=CARTESIAN_POINT('Ctrl Pts',(0.826255568446133,37.2468000776565,2.3601888522854));
#6038=CARTESIAN_POINT('Ctrl Pts',(0.059383723509268,37.3718000776565,2.62865556059567));
#6039=CARTESIAN_POINT('Ctrl Pts',(-0.718829403428604,37.4968000776565,2.39509372919037));
#6040=CARTESIAN_POINT('Ctrl Pts',(-1.49704253036648,37.6218000776565,2.16153189778506));
#6041=CARTESIAN_POINT('Ctrl Pts',(-1.98934597530643,37.7468000776565,1.51515420778634));
#6042=CARTESIAN_POINT('Ctrl Pts',(-2.48164942024637,37.8718000776565,0.868776517787626));
#6043=CARTESIAN_POINT('Ctrl Pts',(-2.5,37.9968000776565,0.0564772772053586));
#6044=CARTESIAN_POINT('Ctrl Pts',(-2.51835057975363,38.1218000776565,-0.755821963376908));
#6045=CARTESIAN_POINT('Ctrl Pts',(-2.05573899656831,38.2468000776565,-1.42377205367602));
#6046=CARTESIAN_POINT('Ctrl Pts',(-1.593127413383,38.3718000776565,-2.09172214397514));
#6047=CARTESIAN_POINT('Ctrl Pts',(-0.826255568446133,38.4968000776565,-2.3601888522854));
#6048=CARTESIAN_POINT('Ctrl Pts',(-0.0593837235092677,38.6218000776565,
-2.62865556059567));
#6049=CARTESIAN_POINT('Ctrl Pts',(0.718829403428605,38.7468000776565,-2.39509372919037));
#6050=CARTESIAN_POINT('Ctrl Pts',(1.49704253036648,38.8718000776565,-2.16153189778506));
#6051=CARTESIAN_POINT('Ctrl Pts',(1.98934597530643,38.9968000776565,-1.51515420778634));
#6052=CARTESIAN_POINT('Ctrl Pts',(2.48164942024637,39.1218000776565,-0.868776517787625));
#6053=CARTESIAN_POINT('Ctrl Pts',(2.5,39.2468000776565,-0.0564772772053589));
#6054=CARTESIAN_POINT('Ctrl Pts',(2.51835057975363,39.3718000776565,0.755821963376907));
#6055=CARTESIAN_POINT('Ctrl Pts',(2.05573899656831,39.4968000776565,1.42377205367602));
#6056=CARTESIAN_POINT('Ctrl Pts',(1.593127413383,39.6218000776565,2.09172214397514));
#6057=CARTESIAN_POINT('Ctrl Pts',(0.826255568446133,39.7468000776565,2.3601888522854));
#6058=CARTESIAN_POINT('Ctrl Pts',(0.059383723509268,39.8718000776565,2.62865556059567));
#6059=CARTESIAN_POINT('Ctrl Pts',(-0.718829403428604,39.9968000776565,2.39509372919037));
#6060=CARTESIAN_POINT('Ctrl Pts',(-1.49704253036648,40.1218000776565,2.16153189778506));
#6061=CARTESIAN_POINT('Ctrl Pts',(-1.98934597530643,40.2468000776565,1.51515420778634));
#6062=CARTESIAN_POINT('Ctrl Pts',(-2.48164942024637,40.3718000776565,0.868776517787626));
#6063=CARTESIAN_POINT('Ctrl Pts',(-2.5,40.4968000776565,0.0564772772053586));
#6064=CARTESIAN_POINT('Ctrl Pts',(-2.5,14.5031999223435,-0.056477277205306));
#6065=CARTESIAN_POINT('Ctrl Pts',(-2.48164942024639,14.6281999223435,-0.868776517787572));
#6066=CARTESIAN_POINT('Ctrl Pts',(-1.98934597530646,14.7531999223435,-1.5151542077863));
#6067=CARTESIAN_POINT('Ctrl Pts',(-1.49704253036652,14.8781999223435,-2.16153189778503));
#6068=CARTESIAN_POINT('Ctrl Pts',(-0.718829403428655,15.0031999223435,-2.39509372919035));
#6069=CARTESIAN_POINT('Ctrl Pts',(0.0593837235092121,15.1281999223435,-2.62865556059567));
#6070=CARTESIAN_POINT('Ctrl Pts',(0.826255568446083,15.2531999223435,-2.36018885228542));
#6071=CARTESIAN_POINT('Ctrl Pts',(1.59312741338295,15.3781999223435,-2.09172214397517));
#6072=CARTESIAN_POINT('Ctrl Pts',(2.05573899656828,15.5031999223436,-1.42377205367607));
#6073=CARTESIAN_POINT('Ctrl Pts',(2.51835057975361,15.6281999223435,-0.755821963376961));
#6074=CARTESIAN_POINT('Ctrl Pts',(2.5,15.7531999223435,0.0564772772053057));
#6075=CARTESIAN_POINT('Ctrl Pts',(2.48164942024639,15.8781999223435,0.868776517787572));
#6076=CARTESIAN_POINT('Ctrl Pts',(1.98934597530646,16.0031999223435,1.5151542077863));
#6077=CARTESIAN_POINT('Ctrl Pts',(1.49704253036652,16.1281999223435,2.16153189778503));
#6078=CARTESIAN_POINT('Ctrl Pts',(0.718829403428655,16.2531999223435,2.39509372919035));
#6079=CARTESIAN_POINT('Ctrl Pts',(-0.0593837235092117,16.3781999223435,
2.62865556059567));
#6080=CARTESIAN_POINT('Ctrl Pts',(-0.826255568446083,16.5031999223435,2.36018885228542));
#6081=CARTESIAN_POINT('Ctrl Pts',(-1.59312741338295,16.6281999223435,2.09172214397517));
#6082=CARTESIAN_POINT('Ctrl Pts',(-2.05573899656828,16.7531999223435,1.42377205367607));
#6083=CARTESIAN_POINT('Ctrl Pts',(-2.51835057975361,16.8781999223435,0.755821963376961));
#6084=CARTESIAN_POINT('Ctrl Pts',(-2.5,17.0031999223435,-0.056477277205306));
#6085=CARTESIAN_POINT('Ctrl Pts',(-2.48164942024639,17.1281999223435,-0.868776517787572));
#6086=CARTESIAN_POINT('Ctrl Pts',(-1.98934597530646,17.2531999223435,-1.5151542077863));
#6087=CARTESIAN_POINT('Ctrl Pts',(-1.49704253036652,17.3781999223435,-2.16153189778503));
#6088=CARTESIAN_POINT('Ctrl Pts',(-0.718829403428655,17.5031999223435,-2.39509372919035));
#6089=CARTESIAN_POINT('Ctrl Pts',(0.0593837235092121,17.6281999223435,-2.62865556059567));
#6090=CARTESIAN_POINT('Ctrl Pts',(0.826255568446083,17.7531999223435,-2.36018885228542));
#6091=CARTESIAN_POINT('Ctrl Pts',(1.59312741338295,17.8781999223435,-2.09172214397517));
#6092=CARTESIAN_POINT('Ctrl Pts',(2.05573899656828,18.0031999223435,-1.42377205367607));
#6093=CARTESIAN_POINT('Ctrl Pts',(2.51835057975361,18.1281999223435,-0.755821963376961));
#6094=CARTESIAN_POINT('Ctrl Pts',(2.5,18.2531999223435,0.0564772772053057));
#6095=CARTESIAN_POINT('Ctrl Pts',(2.48164942024639,18.3781999223435,0.868776517787572));
#6096=CARTESIAN_POINT('Ctrl Pts',(1.98934597530646,18.5031999223435,1.5151542077863));
#6097=CARTESIAN_POINT('Ctrl Pts',(1.49704253036652,18.6281999223435,2.16153189778503));
#6098=CARTESIAN_POINT('Ctrl Pts',(0.718829403428655,18.7531999223435,2.39509372919035));
#6099=CARTESIAN_POINT('Ctrl Pts',(-0.0593837235092117,18.8781999223435,
2.62865556059567));
#6100=CARTESIAN_POINT('Ctrl Pts',(-0.826255568446083,19.0031999223435,2.36018885228542));
#6101=CARTESIAN_POINT('Ctrl Pts',(-1.59312741338295,19.1281999223435,2.09172214397517));
#6102=CARTESIAN_POINT('Ctrl Pts',(-2.05573899656828,19.2531999223435,1.42377205367607));
#6103=CARTESIAN_POINT('Ctrl Pts',(-2.51835057975361,19.3781999223435,0.755821963376961));
#6104=CARTESIAN_POINT('Ctrl Pts',(-2.5,19.5031999223435,-0.056477277205306));
#6105=CARTESIAN_POINT('Ctrl Pts',(-2.48164942024639,19.6281999223435,-0.868776517787572));
#6106=CARTESIAN_POINT('Ctrl Pts',(-1.98934597530646,19.7531999223435,-1.5151542077863));
#6107=CARTESIAN_POINT('Ctrl Pts',(-1.49704253036652,19.8781999223435,-2.16153189778503));
#6108=CARTESIAN_POINT('Ctrl Pts',(-0.718829403428655,20.0031999223435,-2.39509372919035));
#6109=CARTESIAN_POINT('Ctrl Pts',(0.0593837235092121,20.1281999223436,-2.62865556059567));
#6110=CARTESIAN_POINT('Ctrl Pts',(0.826255568446083,20.2531999223435,-2.36018885228542));
#6111=CARTESIAN_POINT('Ctrl Pts',(1.59312741338295,20.3781999223435,-2.09172214397517));
#6112=CARTESIAN_POINT('Ctrl Pts',(2.05573899656828,20.5031999223436,-1.42377205367607));
#6113=CARTESIAN_POINT('Ctrl Pts',(2.51835057975361,20.6281999223435,-0.755821963376961));
#6114=CARTESIAN_POINT('Ctrl Pts',(2.5,20.7531999223436,0.0564772772053057));
#6115=CARTESIAN_POINT('Ctrl Pts',(2.48164942024639,20.8781999223436,0.868776517787572));
#6116=CARTESIAN_POINT('Ctrl Pts',(1.98934597530646,21.0031999223435,1.5151542077863));
#6117=CARTESIAN_POINT('Ctrl Pts',(1.49704253036652,21.1281999223435,2.16153189778503));
#6118=CARTESIAN_POINT('Ctrl Pts',(0.718829403428655,21.2531999223435,2.39509372919035));
#6119=CARTESIAN_POINT('Ctrl Pts',(-0.0593837235092117,21.3781999223435,
2.62865556059567));
#6120=CARTESIAN_POINT('Ctrl Pts',(-0.826255568446083,21.5031999223435,2.36018885228542));
#6121=CARTESIAN_POINT('Ctrl Pts',(-1.59312741338295,21.6281999223435,2.09172214397517));
#6122=CARTESIAN_POINT('Ctrl Pts',(-2.05573899656828,21.7531999223435,1.42377205367607));
#6123=CARTESIAN_POINT('Ctrl Pts',(-2.51835057975361,21.8781999223435,0.755821963376961));
#6124=CARTESIAN_POINT('Ctrl Pts',(-2.5,22.0031999223436,-0.056477277205306));
#6125=CARTESIAN_POINT('Ctrl Pts',(-2.48164942024639,22.1281999223435,-0.868776517787572));
#6126=CARTESIAN_POINT('Ctrl Pts',(-1.98934597530646,22.2531999223435,-1.5151542077863));
#6127=CARTESIAN_POINT('Ctrl Pts',(-1.49704253036652,22.3781999223435,-2.16153189778503));
#6128=CARTESIAN_POINT('Ctrl Pts',(-0.718829403428655,22.5031999223435,-2.39509372919035));
#6129=CARTESIAN_POINT('Ctrl Pts',(0.0593837235092121,22.6281999223436,-2.62865556059567));
#6130=CARTESIAN_POINT('Ctrl Pts',(0.826255568446083,22.7531999223435,-2.36018885228542));
#6131=CARTESIAN_POINT('Ctrl Pts',(1.59312741338295,22.8781999223435,-2.09172214397517));
#6132=CARTESIAN_POINT('Ctrl Pts',(2.05573899656828,23.0031999223435,-1.42377205367607));
#6133=CARTESIAN_POINT('Ctrl Pts',(2.51835057975361,23.1281999223435,-0.755821963376961));
#6134=CARTESIAN_POINT('Ctrl Pts',(2.5,23.2531999223436,0.0564772772053057));
#6135=CARTESIAN_POINT('Ctrl Pts',(2.48164942024639,23.3781999223435,0.868776517787572));
#6136=CARTESIAN_POINT('Ctrl Pts',(1.98934597530646,23.5031999223436,1.5151542077863));
#6137=CARTESIAN_POINT('Ctrl Pts',(1.49704253036652,23.6281999223435,2.16153189778503));
#6138=CARTESIAN_POINT('Ctrl Pts',(0.718829403428655,23.7531999223435,2.39509372919035));
#6139=CARTESIAN_POINT('Ctrl Pts',(-0.0593837235092117,23.8781999223435,
2.62865556059567));
#6140=CARTESIAN_POINT('Ctrl Pts',(-0.826255568446083,24.0031999223435,2.36018885228542));
#6141=CARTESIAN_POINT('Ctrl Pts',(-1.59312741338295,24.1281999223435,2.09172214397517));
#6142=CARTESIAN_POINT('Ctrl Pts',(-2.05573899656828,24.2531999223435,1.42377205367607));
#6143=CARTESIAN_POINT('Ctrl Pts',(-2.51835057975361,24.3781999223435,0.755821963376961));
#6144=CARTESIAN_POINT('Ctrl Pts',(-2.5,24.5031999223436,-0.056477277205306));
#6145=CARTESIAN_POINT('Ctrl Pts',(-2.48164942024639,24.6281999223435,-0.868776517787572));
#6146=CARTESIAN_POINT('Ctrl Pts',(-1.98934597530646,24.7531999223435,-1.5151542077863));
#6147=CARTESIAN_POINT('Ctrl Pts',(-1.49704253036652,24.8781999223436,-2.16153189778503));
#6148=CARTESIAN_POINT('Ctrl Pts',(-0.718829403428655,25.0031999223435,-2.39509372919035));
#6149=CARTESIAN_POINT('Ctrl Pts',(0.0593837235092121,25.1281999223435,-2.62865556059567));
#6150=CARTESIAN_POINT('Ctrl Pts',(0.826255568446083,25.2531999223435,-2.36018885228542));
#6151=CARTESIAN_POINT('Ctrl Pts',(1.59312741338295,25.3781999223435,-2.09172214397517));
#6152=CARTESIAN_POINT('Ctrl Pts',(2.05573899656828,25.5031999223435,-1.42377205367607));
#6153=CARTESIAN_POINT('Ctrl Pts',(2.51835057975361,25.6281999223435,-0.755821963376961));
#6154=CARTESIAN_POINT('Ctrl Pts',(2.5,25.7531999223436,0.0564772772053057));
#6155=CARTESIAN_POINT('Ctrl Pts',(2.48164942024639,25.8781999223436,0.868776517787572));
#6156=CARTESIAN_POINT('Ctrl Pts',(1.98934597530646,26.0031999223435,1.5151542077863));
#6157=CARTESIAN_POINT('Ctrl Pts',(1.49704253036652,26.1281999223435,2.16153189778503));
#6158=CARTESIAN_POINT('Ctrl Pts',(0.718829403428655,26.2531999223435,2.39509372919035));
#6159=CARTESIAN_POINT('Ctrl Pts',(-0.0593837235092117,26.3781999223436,
2.62865556059567));
#6160=CARTESIAN_POINT('Ctrl Pts',(-0.826255568446083,26.5031999223435,2.36018885228542));
#6161=CARTESIAN_POINT('Ctrl Pts',(-1.59312741338295,26.6281999223435,2.09172214397517));
#6162=CARTESIAN_POINT('Ctrl Pts',(-2.05573899656828,26.7531999223436,1.42377205367607));
#6163=CARTESIAN_POINT('Ctrl Pts',(-2.51835057975361,26.8781999223435,0.755821963376961));
#6164=CARTESIAN_POINT('Ctrl Pts',(-2.5,27.0031999223436,-0.056477277205306));
#6165=CARTESIAN_POINT('Ctrl Pts',(-2.48164942024639,27.1281999223436,-0.868776517787572));
#6166=CARTESIAN_POINT('Ctrl Pts',(-1.98934597530646,27.2531999223435,-1.5151542077863));
#6167=CARTESIAN_POINT('Ctrl Pts',(-1.49704253036652,27.3781999223436,-2.16153189778503));
#6168=CARTESIAN_POINT('Ctrl Pts',(-0.718829403428655,27.5031999223435,-2.39509372919035));
#6169=CARTESIAN_POINT('Ctrl Pts',(0.0593837235092121,27.6281999223435,-2.62865556059567));
#6170=CARTESIAN_POINT('Ctrl Pts',(0.826255568446083,27.7531999223436,-2.36018885228542));
#6171=CARTESIAN_POINT('Ctrl Pts',(1.59312741338295,27.8781999223436,-2.09172214397517));
#6172=CARTESIAN_POINT('Ctrl Pts',(2.05573899656828,28.0031999223436,-1.42377205367607));
#6173=CARTESIAN_POINT('Ctrl Pts',(2.51835057975361,28.1281999223436,-0.755821963376961));
#6174=CARTESIAN_POINT('Ctrl Pts',(2.5,28.2531999223436,0.0564772772053057));
#6175=CARTESIAN_POINT('Ctrl Pts',(2.48164942024639,28.3781999223436,0.868776517787572));
#6176=CARTESIAN_POINT('Ctrl Pts',(1.98934597530646,28.5031999223436,1.5151542077863));
#6177=CARTESIAN_POINT('Ctrl Pts',(1.49704253036652,28.6281999223436,2.16153189778503));
#6178=CARTESIAN_POINT('Ctrl Pts',(0.718829403428655,28.7531999223435,2.39509372919035));
#6179=CARTESIAN_POINT('Ctrl Pts',(-0.0593837235092117,28.8781999223435,
2.62865556059567));
#6180=CARTESIAN_POINT('Ctrl Pts',(-0.826255568446083,29.0031999223436,2.36018885228542));
#6181=CARTESIAN_POINT('Ctrl Pts',(-1.59312741338295,29.1281999223435,2.09172214397517));
#6182=CARTESIAN_POINT('Ctrl Pts',(-2.05573899656828,29.2531999223436,1.42377205367607));
#6183=CARTESIAN_POINT('Ctrl Pts',(-2.51835057975361,29.3781999223436,0.755821963376961));
#6184=CARTESIAN_POINT('Ctrl Pts',(-2.5,29.5031999223436,-0.056477277205306));
#6185=CARTESIAN_POINT('Ctrl Pts',(-2.48164942024639,29.6281999223435,-0.868776517787572));
#6186=CARTESIAN_POINT('Ctrl Pts',(-1.98934597530646,29.7531999223435,-1.5151542077863));
#6187=CARTESIAN_POINT('Ctrl Pts',(-1.49704253036652,29.8781999223435,-2.16153189778503));
#6188=CARTESIAN_POINT('Ctrl Pts',(-0.718829403428655,30.0031999223435,-2.39509372919035));
#6189=CARTESIAN_POINT('Ctrl Pts',(0.0593837235092121,30.1281999223435,-2.62865556059567));
#6190=CARTESIAN_POINT('Ctrl Pts',(0.826255568446083,30.2531999223435,-2.36018885228542));
#6191=CARTESIAN_POINT('Ctrl Pts',(1.59312741338295,30.3781999223435,-2.09172214397517));
#6192=CARTESIAN_POINT('Ctrl Pts',(2.05573899656828,30.5031999223436,-1.42377205367607));
#6193=CARTESIAN_POINT('Ctrl Pts',(2.51835057975361,30.6281999223436,-0.755821963376961));
#6194=CARTESIAN_POINT('Ctrl Pts',(2.5,30.7531999223435,0.0564772772053057));
#6195=CARTESIAN_POINT('Ctrl Pts',(2.48164942024639,30.8781999223435,0.868776517787572));
#6196=CARTESIAN_POINT('Ctrl Pts',(1.98934597530646,31.0031999223436,1.5151542077863));
#6197=CARTESIAN_POINT('Ctrl Pts',(1.49704253036652,31.1281999223435,2.16153189778503));
#6198=CARTESIAN_POINT('Ctrl Pts',(0.718829403428655,31.2531999223435,2.39509372919035));
#6199=CARTESIAN_POINT('Ctrl Pts',(-0.0593837235092117,31.3781999223435,
2.62865556059567));
#6200=CARTESIAN_POINT('Ctrl Pts',(-0.826255568446083,31.5031999223435,2.36018885228542));
#6201=CARTESIAN_POINT('Ctrl Pts',(-1.59312741338295,31.6281999223435,2.09172214397517));
#6202=CARTESIAN_POINT('Ctrl Pts',(-2.05573899656828,31.7531999223436,1.42377205367607));
#6203=CARTESIAN_POINT('Ctrl Pts',(-2.51835057975361,31.8781999223435,0.755821963376961));
#6204=CARTESIAN_POINT('Ctrl Pts',(-2.5,32.0031999223435,-0.056477277205306));
#6205=CARTESIAN_POINT('Ctrl Pts',(-2.48164942024639,32.1281999223435,-0.868776517787572));
#6206=CARTESIAN_POINT('Ctrl Pts',(-1.98934597530646,32.2531999223435,-1.5151542077863));
#6207=CARTESIAN_POINT('Ctrl Pts',(-1.49704253036652,32.3781999223435,-2.16153189778503));
#6208=CARTESIAN_POINT('Ctrl Pts',(-0.718829403428655,32.5031999223435,-2.39509372919035));
#6209=CARTESIAN_POINT('Ctrl Pts',(0.0593837235092121,32.6281999223435,-2.62865556059567));
#6210=CARTESIAN_POINT('Ctrl Pts',(0.826255568446083,32.7531999223435,-2.36018885228542));
#6211=CARTESIAN_POINT('Ctrl Pts',(1.59312741338295,32.8781999223435,-2.09172214397517));
#6212=CARTESIAN_POINT('Ctrl Pts',(2.05573899656828,33.0031999223436,-1.42377205367607));
#6213=CARTESIAN_POINT('Ctrl Pts',(2.51835057975361,33.1281999223435,-0.755821963376961));
#6214=CARTESIAN_POINT('Ctrl Pts',(2.5,33.2531999223435,0.0564772772053057));
#6215=CARTESIAN_POINT('Ctrl Pts',(2.48164942024639,33.3781999223435,0.868776517787572));
#6216=CARTESIAN_POINT('Ctrl Pts',(1.98934597530646,33.5031999223435,1.5151542077863));
#6217=CARTESIAN_POINT('Ctrl Pts',(1.49704253036652,33.6281999223436,2.16153189778503));
#6218=CARTESIAN_POINT('Ctrl Pts',(0.718829403428655,33.7531999223435,2.39509372919035));
#6219=CARTESIAN_POINT('Ctrl Pts',(-0.0593837235092117,33.8781999223435,
2.62865556059567));
#6220=CARTESIAN_POINT('Ctrl Pts',(-0.826255568446083,34.0031999223435,2.36018885228542));
#6221=CARTESIAN_POINT('Ctrl Pts',(-1.59312741338295,34.1281999223435,2.09172214397517));
#6222=CARTESIAN_POINT('Ctrl Pts',(-2.05573899656828,34.2531999223435,1.42377205367607));
#6223=CARTESIAN_POINT('Ctrl Pts',(-2.51835057975361,34.3781999223435,0.755821963376961));
#6224=CARTESIAN_POINT('Ctrl Pts',(-2.5,34.5031999223435,-0.056477277205306));
#6225=CARTESIAN_POINT('Ctrl Pts',(-2.48164942024639,34.6281999223435,-0.868776517787572));
#6226=CARTESIAN_POINT('Ctrl Pts',(-1.98934597530646,34.7531999223435,-1.5151542077863));
#6227=CARTESIAN_POINT('Ctrl Pts',(-1.49704253036652,34.8781999223436,-2.16153189778503));
#6228=CARTESIAN_POINT('Ctrl Pts',(-0.718829403428655,35.0031999223435,-2.39509372919035));
#6229=CARTESIAN_POINT('Ctrl Pts',(0.0593837235092121,35.1281999223435,-2.62865556059567));
#6230=CARTESIAN_POINT('Ctrl Pts',(0.826255568446083,35.2531999223435,-2.36018885228542));
#6231=CARTESIAN_POINT('Ctrl Pts',(1.59312741338295,35.3781999223435,-2.09172214397517));
#6232=CARTESIAN_POINT('Ctrl Pts',(2.05573899656828,35.5031999223436,-1.42377205367607));
#6233=CARTESIAN_POINT('Ctrl Pts',(2.51835057975361,35.6281999223435,-0.755821963376961));
#6234=CARTESIAN_POINT('Ctrl Pts',(2.5,35.7531999223435,0.0564772772053057));
#6235=CARTESIAN_POINT('Ctrl Pts',(2.48164942024639,35.8781999223435,0.868776517787572));
#6236=CARTESIAN_POINT('Ctrl Pts',(1.98934597530646,36.0031999223435,1.5151542077863));
#6237=CARTESIAN_POINT('Ctrl Pts',(1.49704253036652,36.1281999223436,2.16153189778503));
#6238=CARTESIAN_POINT('Ctrl Pts',(0.718829403428655,36.2531999223435,2.39509372919035));
#6239=CARTESIAN_POINT('Ctrl Pts',(-0.0593837235092117,36.3781999223435,
2.62865556059567));
#6240=CARTESIAN_POINT('Ctrl Pts',(-0.826255568446083,36.5031999223435,2.36018885228542));
#6241=CARTESIAN_POINT('Ctrl Pts',(-1.59312741338295,36.6281999223435,2.09172214397517));
#6242=CARTESIAN_POINT('Ctrl Pts',(-2.05573899656828,36.7531999223436,1.42377205367607));
#6243=CARTESIAN_POINT('Ctrl Pts',(-2.51835057975361,36.8781999223435,0.755821963376961));
#6244=CARTESIAN_POINT('Ctrl Pts',(-2.5,37.0031999223435,-0.056477277205306));
#6245=CARTESIAN_POINT('Ctrl Pts',(-2.48164942024639,37.1281999223435,-0.868776517787572));
#6246=CARTESIAN_POINT('Ctrl Pts',(-1.98934597530646,37.2531999223435,-1.5151542077863));
#6247=CARTESIAN_POINT('Ctrl Pts',(-1.49704253036652,37.3781999223436,-2.16153189778503));
#6248=CARTESIAN_POINT('Ctrl Pts',(-0.718829403428655,37.5031999223435,-2.39509372919035));
#6249=CARTESIAN_POINT('Ctrl Pts',(0.0593837235092121,37.6281999223435,-2.62865556059567));
#6250=CARTESIAN_POINT('Ctrl Pts',(0.826255568446083,37.7531999223435,-2.36018885228542));
#6251=CARTESIAN_POINT('Ctrl Pts',(1.59312741338295,37.8781999223435,-2.09172214397517));
#6252=CARTESIAN_POINT('Ctrl Pts',(2.05573899656828,38.0031999223435,-1.42377205367607));
#6253=CARTESIAN_POINT('Ctrl Pts',(2.51835057975361,38.1281999223435,-0.755821963376961));
#6254=CARTESIAN_POINT('Ctrl Pts',(2.5,38.2531999223435,0.0564772772053057));
#6255=CARTESIAN_POINT('Ctrl Pts',(2.48164942024639,38.3781999223435,0.868776517787572));
#6256=CARTESIAN_POINT('Ctrl Pts',(1.98934597530646,38.5031999223435,1.5151542077863));
#6257=CARTESIAN_POINT('Ctrl Pts',(1.49704253036652,38.6281999223436,2.16153189778503));
#6258=CARTESIAN_POINT('Ctrl Pts',(0.718829403428655,38.7531999223435,2.39509372919035));
#6259=CARTESIAN_POINT('Ctrl Pts',(-0.0593837235092117,38.8781999223435,
2.62865556059567));
#6260=CARTESIAN_POINT('Ctrl Pts',(-0.826255568446083,39.0031999223436,2.36018885228542));
#6261=CARTESIAN_POINT('Ctrl Pts',(-1.59312741338295,39.1281999223435,2.09172214397517));
#6262=CARTESIAN_POINT('Ctrl Pts',(-2.05573899656828,39.2531999223436,1.42377205367607));
#6263=CARTESIAN_POINT('Ctrl Pts',(-2.51835057975361,39.3781999223435,0.755821963376961));
#6264=CARTESIAN_POINT('Ctrl Pts',(-2.5,39.5031999223436,-0.056477277205306));
#6265=CARTESIAN_POINT('Ctrl Pts',(-3.5,14.5031999223435,-0.0564772772052956));
#6266=CARTESIAN_POINT('Ctrl Pts',(-3.48164942024639,14.6281999223435,-1.19369621402047));
#6267=CARTESIAN_POINT('Ctrl Pts',(-2.79836296968141,14.7531999223435,-2.10293946007877));
#6268=CARTESIAN_POINT('Ctrl Pts',(-2.11507651911643,14.8781999223435,-3.01218270613706));
#6269=CARTESIAN_POINT('Ctrl Pts',(-1.02784639780361,15.0031999223435,-3.3461502454855));
#6270=CARTESIAN_POINT('Ctrl Pts',(0.0593837235092011,15.1281999223435,-3.68011778483394));
#6271=CARTESIAN_POINT('Ctrl Pts',(1.13527256282102,15.2531999223435,-3.31124536858058));
#6272=CARTESIAN_POINT('Ctrl Pts',(2.21116140213284,15.3781999223435,-2.94237295232722));
#6273=CARTESIAN_POINT('Ctrl Pts',(2.86475599094322,15.5031999223435,-2.01155730596855));
#6274=CARTESIAN_POINT('Ctrl Pts',(3.51835057975361,15.6281999223435,-1.08074165960988));
#6275=CARTESIAN_POINT('Ctrl Pts',(3.5,15.7531999223435,0.0564772772052952));
#6276=CARTESIAN_POINT('Ctrl Pts',(3.48164942024639,15.8781999223435,1.19369621402047));
#6277=CARTESIAN_POINT('Ctrl Pts',(2.79836296968141,16.0031999223435,2.10293946007876));
#6278=CARTESIAN_POINT('Ctrl Pts',(2.11507651911643,16.1281999223435,3.01218270613706));
#6279=CARTESIAN_POINT('Ctrl Pts',(1.02784639780361,16.2531999223435,3.3461502454855));
#6280=CARTESIAN_POINT('Ctrl Pts',(-0.0593837235092006,16.3781999223435,
3.68011778483394));
#6281=CARTESIAN_POINT('Ctrl Pts',(-1.13527256282102,16.5031999223435,3.31124536858058));
#6282=CARTESIAN_POINT('Ctrl Pts',(-2.21116140213284,16.6281999223435,2.94237295232722));
#6283=CARTESIAN_POINT('Ctrl Pts',(-2.86475599094322,16.7531999223435,2.01155730596855));
#6284=CARTESIAN_POINT('Ctrl Pts',(-3.51835057975361,16.8781999223435,1.08074165960988));
#6285=CARTESIAN_POINT('Ctrl Pts',(-3.5,17.0031999223435,-0.0564772772052956));
#6286=CARTESIAN_POINT('Ctrl Pts',(-3.48164942024639,17.1281999223435,-1.19369621402047));
#6287=CARTESIAN_POINT('Ctrl Pts',(-2.79836296968141,17.2531999223435,-2.10293946007877));
#6288=CARTESIAN_POINT('Ctrl Pts',(-2.11507651911643,17.3781999223435,-3.01218270613706));
#6289=CARTESIAN_POINT('Ctrl Pts',(-1.02784639780361,17.5031999223435,-3.3461502454855));
#6290=CARTESIAN_POINT('Ctrl Pts',(0.0593837235092011,17.6281999223435,-3.68011778483394));
#6291=CARTESIAN_POINT('Ctrl Pts',(1.13527256282102,17.7531999223435,-3.31124536858058));
#6292=CARTESIAN_POINT('Ctrl Pts',(2.21116140213284,17.8781999223435,-2.94237295232722));
#6293=CARTESIAN_POINT('Ctrl Pts',(2.86475599094322,18.0031999223435,-2.01155730596855));
#6294=CARTESIAN_POINT('Ctrl Pts',(3.51835057975361,18.1281999223435,-1.08074165960988));
#6295=CARTESIAN_POINT('Ctrl Pts',(3.5,18.2531999223435,0.0564772772052952));
#6296=CARTESIAN_POINT('Ctrl Pts',(3.48164942024639,18.3781999223435,1.19369621402047));
#6297=CARTESIAN_POINT('Ctrl Pts',(2.79836296968141,18.5031999223435,2.10293946007876));
#6298=CARTESIAN_POINT('Ctrl Pts',(2.11507651911643,18.6281999223435,3.01218270613706));
#6299=CARTESIAN_POINT('Ctrl Pts',(1.02784639780361,18.7531999223435,3.3461502454855));
#6300=CARTESIAN_POINT('Ctrl Pts',(-0.0593837235092006,18.8781999223435,
3.68011778483394));
#6301=CARTESIAN_POINT('Ctrl Pts',(-1.13527256282102,19.0031999223435,3.31124536858058));
#6302=CARTESIAN_POINT('Ctrl Pts',(-2.21116140213284,19.1281999223435,2.94237295232722));
#6303=CARTESIAN_POINT('Ctrl Pts',(-2.86475599094322,19.2531999223435,2.01155730596855));
#6304=CARTESIAN_POINT('Ctrl Pts',(-3.51835057975361,19.3781999223435,1.08074165960988));
#6305=CARTESIAN_POINT('Ctrl Pts',(-3.5,19.5031999223435,-0.0564772772052956));
#6306=CARTESIAN_POINT('Ctrl Pts',(-3.48164942024639,19.6281999223435,-1.19369621402047));
#6307=CARTESIAN_POINT('Ctrl Pts',(-2.79836296968141,19.7531999223435,-2.10293946007877));
#6308=CARTESIAN_POINT('Ctrl Pts',(-2.11507651911643,19.8781999223435,-3.01218270613706));
#6309=CARTESIAN_POINT('Ctrl Pts',(-1.02784639780361,20.0031999223435,-3.3461502454855));
#6310=CARTESIAN_POINT('Ctrl Pts',(0.0593837235092011,20.1281999223435,-3.68011778483394));
#6311=CARTESIAN_POINT('Ctrl Pts',(1.13527256282102,20.2531999223435,-3.31124536858058));
#6312=CARTESIAN_POINT('Ctrl Pts',(2.21116140213284,20.3781999223435,-2.94237295232722));
#6313=CARTESIAN_POINT('Ctrl Pts',(2.86475599094322,20.5031999223435,-2.01155730596855));
#6314=CARTESIAN_POINT('Ctrl Pts',(3.51835057975361,20.6281999223435,-1.08074165960988));
#6315=CARTESIAN_POINT('Ctrl Pts',(3.5,20.7531999223435,0.0564772772052952));
#6316=CARTESIAN_POINT('Ctrl Pts',(3.48164942024639,20.8781999223435,1.19369621402047));
#6317=CARTESIAN_POINT('Ctrl Pts',(2.79836296968141,21.0031999223435,2.10293946007876));
#6318=CARTESIAN_POINT('Ctrl Pts',(2.11507651911643,21.1281999223435,3.01218270613706));
#6319=CARTESIAN_POINT('Ctrl Pts',(1.02784639780361,21.2531999223435,3.3461502454855));
#6320=CARTESIAN_POINT('Ctrl Pts',(-0.0593837235092006,21.3781999223435,
3.68011778483394));
#6321=CARTESIAN_POINT('Ctrl Pts',(-1.13527256282102,21.5031999223435,3.31124536858058));
#6322=CARTESIAN_POINT('Ctrl Pts',(-2.21116140213284,21.6281999223435,2.94237295232722));
#6323=CARTESIAN_POINT('Ctrl Pts',(-2.86475599094322,21.7531999223435,2.01155730596855));
#6324=CARTESIAN_POINT('Ctrl Pts',(-3.51835057975361,21.8781999223435,1.08074165960988));
#6325=CARTESIAN_POINT('Ctrl Pts',(-3.5,22.0031999223435,-0.0564772772052956));
#6326=CARTESIAN_POINT('Ctrl Pts',(-3.48164942024639,22.1281999223435,-1.19369621402047));
#6327=CARTESIAN_POINT('Ctrl Pts',(-2.79836296968141,22.2531999223435,-2.10293946007877));
#6328=CARTESIAN_POINT('Ctrl Pts',(-2.11507651911643,22.3781999223435,-3.01218270613706));
#6329=CARTESIAN_POINT('Ctrl Pts',(-1.02784639780361,22.5031999223435,-3.3461502454855));
#6330=CARTESIAN_POINT('Ctrl Pts',(0.0593837235092011,22.6281999223435,-3.68011778483394));
#6331=CARTESIAN_POINT('Ctrl Pts',(1.13527256282102,22.7531999223435,-3.31124536858058));
#6332=CARTESIAN_POINT('Ctrl Pts',(2.21116140213284,22.8781999223435,-2.94237295232722));
#6333=CARTESIAN_POINT('Ctrl Pts',(2.86475599094322,23.0031999223435,-2.01155730596855));
#6334=CARTESIAN_POINT('Ctrl Pts',(3.51835057975361,23.1281999223435,-1.08074165960988));
#6335=CARTESIAN_POINT('Ctrl Pts',(3.5,23.2531999223435,0.0564772772052952));
#6336=CARTESIAN_POINT('Ctrl Pts',(3.48164942024639,23.3781999223435,1.19369621402047));
#6337=CARTESIAN_POINT('Ctrl Pts',(2.79836296968141,23.5031999223435,2.10293946007876));
#6338=CARTESIAN_POINT('Ctrl Pts',(2.11507651911643,23.6281999223435,3.01218270613706));
#6339=CARTESIAN_POINT('Ctrl Pts',(1.02784639780361,23.7531999223435,3.3461502454855));
#6340=CARTESIAN_POINT('Ctrl Pts',(-0.0593837235092006,23.8781999223435,
3.68011778483394));
#6341=CARTESIAN_POINT('Ctrl Pts',(-1.13527256282102,24.0031999223435,3.31124536858058));
#6342=CARTESIAN_POINT('Ctrl Pts',(-2.21116140213284,24.1281999223435,2.94237295232722));
#6343=CARTESIAN_POINT('Ctrl Pts',(-2.86475599094322,24.2531999223435,2.01155730596855));
#6344=CARTESIAN_POINT('Ctrl Pts',(-3.51835057975361,24.3781999223435,1.08074165960988));
#6345=CARTESIAN_POINT('Ctrl Pts',(-3.5,24.5031999223435,-0.0564772772052956));
#6346=CARTESIAN_POINT('Ctrl Pts',(-3.48164942024639,24.6281999223435,-1.19369621402047));
#6347=CARTESIAN_POINT('Ctrl Pts',(-2.79836296968141,24.7531999223435,-2.10293946007877));
#6348=CARTESIAN_POINT('Ctrl Pts',(-2.11507651911643,24.8781999223436,-3.01218270613706));
#6349=CARTESIAN_POINT('Ctrl Pts',(-1.02784639780361,25.0031999223435,-3.3461502454855));
#6350=CARTESIAN_POINT('Ctrl Pts',(0.0593837235092011,25.1281999223435,-3.68011778483394));
#6351=CARTESIAN_POINT('Ctrl Pts',(1.13527256282102,25.2531999223435,-3.31124536858058));
#6352=CARTESIAN_POINT('Ctrl Pts',(2.21116140213284,25.3781999223435,-2.94237295232722));
#6353=CARTESIAN_POINT('Ctrl Pts',(2.86475599094322,25.5031999223436,-2.01155730596855));
#6354=CARTESIAN_POINT('Ctrl Pts',(3.51835057975361,25.6281999223435,-1.08074165960988));
#6355=CARTESIAN_POINT('Ctrl Pts',(3.5,25.7531999223436,0.0564772772052952));
#6356=CARTESIAN_POINT('Ctrl Pts',(3.48164942024639,25.8781999223435,1.19369621402047));
#6357=CARTESIAN_POINT('Ctrl Pts',(2.79836296968141,26.0031999223435,2.10293946007876));
#6358=CARTESIAN_POINT('Ctrl Pts',(2.11507651911643,26.1281999223436,3.01218270613706));
#6359=CARTESIAN_POINT('Ctrl Pts',(1.02784639780361,26.2531999223435,3.3461502454855));
#6360=CARTESIAN_POINT('Ctrl Pts',(-0.0593837235092006,26.3781999223435,
3.68011778483394));
#6361=CARTESIAN_POINT('Ctrl Pts',(-1.13527256282102,26.5031999223435,3.31124536858058));
#6362=CARTESIAN_POINT('Ctrl Pts',(-2.21116140213284,26.6281999223435,2.94237295232722));
#6363=CARTESIAN_POINT('Ctrl Pts',(-2.86475599094322,26.7531999223436,2.01155730596855));
#6364=CARTESIAN_POINT('Ctrl Pts',(-3.51835057975361,26.8781999223435,1.08074165960988));
#6365=CARTESIAN_POINT('Ctrl Pts',(-3.5,27.0031999223436,-0.0564772772052956));
#6366=CARTESIAN_POINT('Ctrl Pts',(-3.48164942024639,27.1281999223435,-1.19369621402047));
#6367=CARTESIAN_POINT('Ctrl Pts',(-2.79836296968141,27.2531999223435,-2.10293946007877));
#6368=CARTESIAN_POINT('Ctrl Pts',(-2.11507651911643,27.3781999223436,-3.01218270613706));
#6369=CARTESIAN_POINT('Ctrl Pts',(-1.02784639780361,27.5031999223435,-3.3461502454855));
#6370=CARTESIAN_POINT('Ctrl Pts',(0.0593837235092011,27.6281999223435,-3.68011778483394));
#6371=CARTESIAN_POINT('Ctrl Pts',(1.13527256282102,27.7531999223435,-3.31124536858058));
#6372=CARTESIAN_POINT('Ctrl Pts',(2.21116140213284,27.8781999223435,-2.94237295232722));
#6373=CARTESIAN_POINT('Ctrl Pts',(2.86475599094322,28.0031999223435,-2.01155730596855));
#6374=CARTESIAN_POINT('Ctrl Pts',(3.51835057975361,28.1281999223435,-1.08074165960988));
#6375=CARTESIAN_POINT('Ctrl Pts',(3.5,28.2531999223435,0.0564772772052952));
#6376=CARTESIAN_POINT('Ctrl Pts',(3.48164942024639,28.3781999223435,1.19369621402047));
#6377=CARTESIAN_POINT('Ctrl Pts',(2.79836296968141,28.5031999223435,2.10293946007876));
#6378=CARTESIAN_POINT('Ctrl Pts',(2.11507651911643,28.6281999223435,3.01218270613706));
#6379=CARTESIAN_POINT('Ctrl Pts',(1.02784639780361,28.7531999223435,3.3461502454855));
#6380=CARTESIAN_POINT('Ctrl Pts',(-0.0593837235092006,28.8781999223435,
3.68011778483394));
#6381=CARTESIAN_POINT('Ctrl Pts',(-1.13527256282102,29.0031999223435,3.31124536858058));
#6382=CARTESIAN_POINT('Ctrl Pts',(-2.21116140213284,29.1281999223435,2.94237295232722));
#6383=CARTESIAN_POINT('Ctrl Pts',(-2.86475599094322,29.2531999223435,2.01155730596855));
#6384=CARTESIAN_POINT('Ctrl Pts',(-3.51835057975361,29.3781999223435,1.08074165960988));
#6385=CARTESIAN_POINT('Ctrl Pts',(-3.5,29.5031999223435,-0.0564772772052956));
#6386=CARTESIAN_POINT('Ctrl Pts',(-3.48164942024639,29.6281999223435,-1.19369621402047));
#6387=CARTESIAN_POINT('Ctrl Pts',(-2.79836296968141,29.7531999223435,-2.10293946007877));
#6388=CARTESIAN_POINT('Ctrl Pts',(-2.11507651911643,29.8781999223435,-3.01218270613706));
#6389=CARTESIAN_POINT('Ctrl Pts',(-1.02784639780361,30.0031999223435,-3.3461502454855));
#6390=CARTESIAN_POINT('Ctrl Pts',(0.0593837235092011,30.1281999223435,-3.68011778483394));
#6391=CARTESIAN_POINT('Ctrl Pts',(1.13527256282102,30.2531999223435,-3.31124536858058));
#6392=CARTESIAN_POINT('Ctrl Pts',(2.21116140213284,30.3781999223435,-2.94237295232722));
#6393=CARTESIAN_POINT('Ctrl Pts',(2.86475599094322,30.5031999223435,-2.01155730596855));
#6394=CARTESIAN_POINT('Ctrl Pts',(3.51835057975361,30.6281999223435,-1.08074165960988));
#6395=CARTESIAN_POINT('Ctrl Pts',(3.5,30.7531999223435,0.0564772772052952));
#6396=CARTESIAN_POINT('Ctrl Pts',(3.48164942024639,30.8781999223435,1.19369621402047));
#6397=CARTESIAN_POINT('Ctrl Pts',(2.79836296968141,31.0031999223435,2.10293946007876));
#6398=CARTESIAN_POINT('Ctrl Pts',(2.11507651911643,31.1281999223435,3.01218270613706));
#6399=CARTESIAN_POINT('Ctrl Pts',(1.02784639780361,31.2531999223435,3.3461502454855));
#6400=CARTESIAN_POINT('Ctrl Pts',(-0.0593837235092006,31.3781999223435,
3.68011778483394));
#6401=CARTESIAN_POINT('Ctrl Pts',(-1.13527256282102,31.5031999223435,3.31124536858058));
#6402=CARTESIAN_POINT('Ctrl Pts',(-2.21116140213284,31.6281999223435,2.94237295232722));
#6403=CARTESIAN_POINT('Ctrl Pts',(-2.86475599094322,31.7531999223435,2.01155730596855));
#6404=CARTESIAN_POINT('Ctrl Pts',(-3.51835057975361,31.8781999223435,1.08074165960988));
#6405=CARTESIAN_POINT('Ctrl Pts',(-3.5,32.0031999223435,-0.0564772772052956));
#6406=CARTESIAN_POINT('Ctrl Pts',(-3.48164942024639,32.1281999223435,-1.19369621402047));
#6407=CARTESIAN_POINT('Ctrl Pts',(-2.79836296968141,32.2531999223435,-2.10293946007877));
#6408=CARTESIAN_POINT('Ctrl Pts',(-2.11507651911643,32.3781999223436,-3.01218270613706));
#6409=CARTESIAN_POINT('Ctrl Pts',(-1.02784639780361,32.5031999223435,-3.3461502454855));
#6410=CARTESIAN_POINT('Ctrl Pts',(0.0593837235092011,32.6281999223435,-3.68011778483394));
#6411=CARTESIAN_POINT('Ctrl Pts',(1.13527256282102,32.7531999223435,-3.31124536858058));
#6412=CARTESIAN_POINT('Ctrl Pts',(2.21116140213284,32.8781999223435,-2.94237295232722));
#6413=CARTESIAN_POINT('Ctrl Pts',(2.86475599094322,33.0031999223436,-2.01155730596855));
#6414=CARTESIAN_POINT('Ctrl Pts',(3.51835057975361,33.1281999223435,-1.08074165960988));
#6415=CARTESIAN_POINT('Ctrl Pts',(3.5,33.2531999223435,0.0564772772052952));
#6416=CARTESIAN_POINT('Ctrl Pts',(3.48164942024639,33.3781999223435,1.19369621402047));
#6417=CARTESIAN_POINT('Ctrl Pts',(2.79836296968141,33.5031999223435,2.10293946007876));
#6418=CARTESIAN_POINT('Ctrl Pts',(2.11507651911643,33.6281999223435,3.01218270613706));
#6419=CARTESIAN_POINT('Ctrl Pts',(1.02784639780361,33.7531999223435,3.3461502454855));
#6420=CARTESIAN_POINT('Ctrl Pts',(-0.0593837235092006,33.8781999223435,
3.68011778483394));
#6421=CARTESIAN_POINT('Ctrl Pts',(-1.13527256282102,34.0031999223435,3.31124536858058));
#6422=CARTESIAN_POINT('Ctrl Pts',(-2.21116140213284,34.1281999223436,2.94237295232722));
#6423=CARTESIAN_POINT('Ctrl Pts',(-2.86475599094322,34.2531999223436,2.01155730596855));
#6424=CARTESIAN_POINT('Ctrl Pts',(-3.51835057975361,34.3781999223435,1.08074165960988));
#6425=CARTESIAN_POINT('Ctrl Pts',(-3.5,34.5031999223435,-0.0564772772052956));
#6426=CARTESIAN_POINT('Ctrl Pts',(-3.48164942024639,34.6281999223435,-1.19369621402047));
#6427=CARTESIAN_POINT('Ctrl Pts',(-2.79836296968141,34.7531999223435,-2.10293946007877));
#6428=CARTESIAN_POINT('Ctrl Pts',(-2.11507651911643,34.8781999223436,-3.01218270613706));
#6429=CARTESIAN_POINT('Ctrl Pts',(-1.02784639780361,35.0031999223435,-3.3461502454855));
#6430=CARTESIAN_POINT('Ctrl Pts',(0.0593837235092011,35.1281999223435,-3.68011778483394));
#6431=CARTESIAN_POINT('Ctrl Pts',(1.13527256282102,35.2531999223435,-3.31124536858058));
#6432=CARTESIAN_POINT('Ctrl Pts',(2.21116140213284,35.3781999223435,-2.94237295232722));
#6433=CARTESIAN_POINT('Ctrl Pts',(2.86475599094322,35.5031999223436,-2.01155730596855));
#6434=CARTESIAN_POINT('Ctrl Pts',(3.51835057975361,35.6281999223435,-1.08074165960988));
#6435=CARTESIAN_POINT('Ctrl Pts',(3.5,35.7531999223435,0.0564772772052952));
#6436=CARTESIAN_POINT('Ctrl Pts',(3.48164942024639,35.8781999223435,1.19369621402047));
#6437=CARTESIAN_POINT('Ctrl Pts',(2.79836296968141,36.0031999223435,2.10293946007876));
#6438=CARTESIAN_POINT('Ctrl Pts',(2.11507651911643,36.1281999223436,3.01218270613706));
#6439=CARTESIAN_POINT('Ctrl Pts',(1.02784639780361,36.2531999223435,3.3461502454855));
#6440=CARTESIAN_POINT('Ctrl Pts',(-0.0593837235092006,36.3781999223436,
3.68011778483394));
#6441=CARTESIAN_POINT('Ctrl Pts',(-1.13527256282102,36.5031999223435,3.31124536858058));
#6442=CARTESIAN_POINT('Ctrl Pts',(-2.21116140213284,36.6281999223435,2.94237295232722));
#6443=CARTESIAN_POINT('Ctrl Pts',(-2.86475599094322,36.7531999223435,2.01155730596855));
#6444=CARTESIAN_POINT('Ctrl Pts',(-3.51835057975361,36.8781999223435,1.08074165960988));
#6445=CARTESIAN_POINT('Ctrl Pts',(-3.5,37.0031999223435,-0.0564772772052956));
#6446=CARTESIAN_POINT('Ctrl Pts',(-3.48164942024639,37.1281999223435,-1.19369621402047));
#6447=CARTESIAN_POINT('Ctrl Pts',(-2.79836296968141,37.2531999223435,-2.10293946007877));
#6448=CARTESIAN_POINT('Ctrl Pts',(-2.11507651911643,37.3781999223435,-3.01218270613706));
#6449=CARTESIAN_POINT('Ctrl Pts',(-1.02784639780361,37.5031999223435,-3.3461502454855));
#6450=CARTESIAN_POINT('Ctrl Pts',(0.0593837235092011,37.6281999223435,-3.68011778483394));
#6451=CARTESIAN_POINT('Ctrl Pts',(1.13527256282102,37.7531999223435,-3.31124536858058));
#6452=CARTESIAN_POINT('Ctrl Pts',(2.21116140213284,37.8781999223435,-2.94237295232722));
#6453=CARTESIAN_POINT('Ctrl Pts',(2.86475599094322,38.0031999223435,-2.01155730596855));
#6454=CARTESIAN_POINT('Ctrl Pts',(3.51835057975361,38.1281999223435,-1.08074165960988));
#6455=CARTESIAN_POINT('Ctrl Pts',(3.5,38.2531999223435,0.0564772772052952));
#6456=CARTESIAN_POINT('Ctrl Pts',(3.48164942024639,38.3781999223435,1.19369621402047));
#6457=CARTESIAN_POINT('Ctrl Pts',(2.79836296968141,38.5031999223435,2.10293946007876));
#6458=CARTESIAN_POINT('Ctrl Pts',(2.11507651911643,38.6281999223436,3.01218270613706));
#6459=CARTESIAN_POINT('Ctrl Pts',(1.02784639780361,38.7531999223435,3.3461502454855));
#6460=CARTESIAN_POINT('Ctrl Pts',(-0.0593837235092006,38.8781999223435,
3.68011778483394));
#6461=CARTESIAN_POINT('Ctrl Pts',(-1.13527256282102,39.0031999223435,3.31124536858058));
#6462=CARTESIAN_POINT('Ctrl Pts',(-2.21116140213284,39.1281999223435,2.94237295232722));
#6463=CARTESIAN_POINT('Ctrl Pts',(-2.86475599094322,39.2531999223436,2.01155730596855));
#6464=CARTESIAN_POINT('Ctrl Pts',(-3.51835057975361,39.3781999223435,1.08074165960988));
#6465=CARTESIAN_POINT('Ctrl Pts',(-3.5,39.5031999223435,-0.0564772772052956));
#6466=CARTESIAN_POINT('Ctrl Pts',(-4.5,14.5031999223435,-0.0564772772052853));
#6467=CARTESIAN_POINT('Ctrl Pts',(-4.4816494202464,14.6281999223435,-1.51861591025336));
#6468=CARTESIAN_POINT('Ctrl Pts',(-3.60737996405636,14.7531999223435,-2.69072471237123));
#6469=CARTESIAN_POINT('Ctrl Pts',(-2.73311050786633,14.8781999223435,-3.8628335144891));
#6470=CARTESIAN_POINT('Ctrl Pts',(-1.33686339217857,15.0031999223435,-4.29720676178065));
#6471=CARTESIAN_POINT('Ctrl Pts',(0.0593837235091902,15.1281999223435,-4.7315800090722));
#6472=CARTESIAN_POINT('Ctrl Pts',(1.44428955719596,15.2531999223435,-4.26230188487573));
#6473=CARTESIAN_POINT('Ctrl Pts',(2.82919539088272,15.3781999223435,-3.79302376067926));
#6474=CARTESIAN_POINT('Ctrl Pts',(3.67377298531816,15.5031999223435,-2.59934255826103));
#6475=CARTESIAN_POINT('Ctrl Pts',(4.5183505797536,15.6281999223435,-1.40566135584279));
#6476=CARTESIAN_POINT('Ctrl Pts',(4.5,15.7531999223435,0.0564772772052848));
#6477=CARTESIAN_POINT('Ctrl Pts',(4.4816494202464,15.8781999223435,1.51861591025336));
#6478=CARTESIAN_POINT('Ctrl Pts',(3.60737996405636,16.0031999223435,2.69072471237123));
#6479=CARTESIAN_POINT('Ctrl Pts',(2.73311050786633,16.1281999223435,3.8628335144891));
#6480=CARTESIAN_POINT('Ctrl Pts',(1.33686339217857,16.2531999223435,4.29720676178065));
#6481=CARTESIAN_POINT('Ctrl Pts',(-0.0593837235091896,16.3781999223435,
4.7315800090722));
#6482=CARTESIAN_POINT('Ctrl Pts',(-1.44428955719596,16.5031999223435,4.26230188487573));
#6483=CARTESIAN_POINT('Ctrl Pts',(-2.82919539088272,16.6281999223435,3.79302376067927));
#6484=CARTESIAN_POINT('Ctrl Pts',(-3.67377298531816,16.7531999223435,2.59934255826103));
#6485=CARTESIAN_POINT('Ctrl Pts',(-4.5183505797536,16.8781999223435,1.40566135584279));
#6486=CARTESIAN_POINT('Ctrl Pts',(-4.5,17.0031999223435,-0.0564772772052853));
#6487=CARTESIAN_POINT('Ctrl Pts',(-4.4816494202464,17.1281999223435,-1.51861591025336));
#6488=CARTESIAN_POINT('Ctrl Pts',(-3.60737996405636,17.2531999223435,-2.69072471237123));
#6489=CARTESIAN_POINT('Ctrl Pts',(-2.73311050786633,17.3781999223435,-3.8628335144891));
#6490=CARTESIAN_POINT('Ctrl Pts',(-1.33686339217857,17.5031999223435,-4.29720676178065));
#6491=CARTESIAN_POINT('Ctrl Pts',(0.0593837235091902,17.6281999223435,-4.7315800090722));
#6492=CARTESIAN_POINT('Ctrl Pts',(1.44428955719596,17.7531999223435,-4.26230188487573));
#6493=CARTESIAN_POINT('Ctrl Pts',(2.82919539088272,17.8781999223435,-3.79302376067926));
#6494=CARTESIAN_POINT('Ctrl Pts',(3.67377298531816,18.0031999223435,-2.59934255826103));
#6495=CARTESIAN_POINT('Ctrl Pts',(4.5183505797536,18.1281999223435,-1.40566135584279));
#6496=CARTESIAN_POINT('Ctrl Pts',(4.5,18.2531999223435,0.0564772772052848));
#6497=CARTESIAN_POINT('Ctrl Pts',(4.4816494202464,18.3781999223435,1.51861591025336));
#6498=CARTESIAN_POINT('Ctrl Pts',(3.60737996405636,18.5031999223435,2.69072471237123));
#6499=CARTESIAN_POINT('Ctrl Pts',(2.73311050786633,18.6281999223435,3.8628335144891));
#6500=CARTESIAN_POINT('Ctrl Pts',(1.33686339217857,18.7531999223435,4.29720676178065));
#6501=CARTESIAN_POINT('Ctrl Pts',(-0.0593837235091896,18.8781999223435,
4.7315800090722));
#6502=CARTESIAN_POINT('Ctrl Pts',(-1.44428955719596,19.0031999223435,4.26230188487573));
#6503=CARTESIAN_POINT('Ctrl Pts',(-2.82919539088272,19.1281999223435,3.79302376067927));
#6504=CARTESIAN_POINT('Ctrl Pts',(-3.67377298531816,19.2531999223435,2.59934255826103));
#6505=CARTESIAN_POINT('Ctrl Pts',(-4.5183505797536,19.3781999223435,1.40566135584279));
#6506=CARTESIAN_POINT('Ctrl Pts',(-4.5,19.5031999223435,-0.0564772772052853));
#6507=CARTESIAN_POINT('Ctrl Pts',(-4.4816494202464,19.6281999223435,-1.51861591025336));
#6508=CARTESIAN_POINT('Ctrl Pts',(-3.60737996405636,19.7531999223435,-2.69072471237123));
#6509=CARTESIAN_POINT('Ctrl Pts',(-2.73311050786633,19.8781999223435,-3.8628335144891));
#6510=CARTESIAN_POINT('Ctrl Pts',(-1.33686339217857,20.0031999223435,-4.29720676178065));
#6511=CARTESIAN_POINT('Ctrl Pts',(0.0593837235091902,20.1281999223435,-4.7315800090722));
#6512=CARTESIAN_POINT('Ctrl Pts',(1.44428955719596,20.2531999223435,-4.26230188487573));
#6513=CARTESIAN_POINT('Ctrl Pts',(2.82919539088272,20.3781999223435,-3.79302376067926));
#6514=CARTESIAN_POINT('Ctrl Pts',(3.67377298531816,20.5031999223435,-2.59934255826103));
#6515=CARTESIAN_POINT('Ctrl Pts',(4.5183505797536,20.6281999223435,-1.40566135584279));
#6516=CARTESIAN_POINT('Ctrl Pts',(4.5,20.7531999223435,0.0564772772052848));
#6517=CARTESIAN_POINT('Ctrl Pts',(4.4816494202464,20.8781999223435,1.51861591025336));
#6518=CARTESIAN_POINT('Ctrl Pts',(3.60737996405636,21.0031999223435,2.69072471237123));
#6519=CARTESIAN_POINT('Ctrl Pts',(2.73311050786633,21.1281999223435,3.8628335144891));
#6520=CARTESIAN_POINT('Ctrl Pts',(1.33686339217857,21.2531999223435,4.29720676178065));
#6521=CARTESIAN_POINT('Ctrl Pts',(-0.0593837235091896,21.3781999223435,
4.7315800090722));
#6522=CARTESIAN_POINT('Ctrl Pts',(-1.44428955719596,21.5031999223435,4.26230188487573));
#6523=CARTESIAN_POINT('Ctrl Pts',(-2.82919539088272,21.6281999223435,3.79302376067927));
#6524=CARTESIAN_POINT('Ctrl Pts',(-3.67377298531816,21.7531999223435,2.59934255826103));
#6525=CARTESIAN_POINT('Ctrl Pts',(-4.5183505797536,21.8781999223435,1.40566135584279));
#6526=CARTESIAN_POINT('Ctrl Pts',(-4.5,22.0031999223435,-0.0564772772052853));
#6527=CARTESIAN_POINT('Ctrl Pts',(-4.4816494202464,22.1281999223435,-1.51861591025336));
#6528=CARTESIAN_POINT('Ctrl Pts',(-3.60737996405636,22.2531999223435,-2.69072471237123));
#6529=CARTESIAN_POINT('Ctrl Pts',(-2.73311050786633,22.3781999223435,-3.8628335144891));
#6530=CARTESIAN_POINT('Ctrl Pts',(-1.33686339217857,22.5031999223435,-4.29720676178065));
#6531=CARTESIAN_POINT('Ctrl Pts',(0.0593837235091902,22.6281999223435,-4.7315800090722));
#6532=CARTESIAN_POINT('Ctrl Pts',(1.44428955719596,22.7531999223435,-4.26230188487573));
#6533=CARTESIAN_POINT('Ctrl Pts',(2.82919539088272,22.8781999223435,-3.79302376067926));
#6534=CARTESIAN_POINT('Ctrl Pts',(3.67377298531816,23.0031999223435,-2.59934255826103));
#6535=CARTESIAN_POINT('Ctrl Pts',(4.5183505797536,23.1281999223435,-1.40566135584279));
#6536=CARTESIAN_POINT('Ctrl Pts',(4.5,23.2531999223435,0.0564772772052848));
#6537=CARTESIAN_POINT('Ctrl Pts',(4.4816494202464,23.3781999223435,1.51861591025336));
#6538=CARTESIAN_POINT('Ctrl Pts',(3.60737996405636,23.5031999223435,2.69072471237123));
#6539=CARTESIAN_POINT('Ctrl Pts',(2.73311050786633,23.6281999223435,3.8628335144891));
#6540=CARTESIAN_POINT('Ctrl Pts',(1.33686339217857,23.7531999223435,4.29720676178065));
#6541=CARTESIAN_POINT('Ctrl Pts',(-0.0593837235091896,23.8781999223435,
4.7315800090722));
#6542=CARTESIAN_POINT('Ctrl Pts',(-1.44428955719596,24.0031999223435,4.26230188487573));
#6543=CARTESIAN_POINT('Ctrl Pts',(-2.82919539088272,24.1281999223435,3.79302376067927));
#6544=CARTESIAN_POINT('Ctrl Pts',(-3.67377298531816,24.2531999223435,2.59934255826103));
#6545=CARTESIAN_POINT('Ctrl Pts',(-4.5183505797536,24.3781999223435,1.40566135584279));
#6546=CARTESIAN_POINT('Ctrl Pts',(-4.5,24.5031999223436,-0.0564772772052853));
#6547=CARTESIAN_POINT('Ctrl Pts',(-4.4816494202464,24.6281999223435,-1.51861591025336));
#6548=CARTESIAN_POINT('Ctrl Pts',(-3.60737996405636,24.7531999223435,-2.69072471237123));
#6549=CARTESIAN_POINT('Ctrl Pts',(-2.73311050786633,24.8781999223436,-3.8628335144891));
#6550=CARTESIAN_POINT('Ctrl Pts',(-1.33686339217857,25.0031999223435,-4.29720676178065));
#6551=CARTESIAN_POINT('Ctrl Pts',(0.0593837235091902,25.1281999223435,-4.7315800090722));
#6552=CARTESIAN_POINT('Ctrl Pts',(1.44428955719596,25.2531999223435,-4.26230188487573));
#6553=CARTESIAN_POINT('Ctrl Pts',(2.82919539088272,25.3781999223435,-3.79302376067926));
#6554=CARTESIAN_POINT('Ctrl Pts',(3.67377298531816,25.5031999223435,-2.59934255826103));
#6555=CARTESIAN_POINT('Ctrl Pts',(4.5183505797536,25.6281999223435,-1.40566135584279));
#6556=CARTESIAN_POINT('Ctrl Pts',(4.5,25.7531999223436,0.0564772772052848));
#6557=CARTESIAN_POINT('Ctrl Pts',(4.4816494202464,25.8781999223436,1.51861591025336));
#6558=CARTESIAN_POINT('Ctrl Pts',(3.60737996405636,26.0031999223435,2.69072471237123));
#6559=CARTESIAN_POINT('Ctrl Pts',(2.73311050786633,26.1281999223435,3.8628335144891));
#6560=CARTESIAN_POINT('Ctrl Pts',(1.33686339217857,26.2531999223435,4.29720676178065));
#6561=CARTESIAN_POINT('Ctrl Pts',(-0.0593837235091896,26.3781999223436,
4.7315800090722));
#6562=CARTESIAN_POINT('Ctrl Pts',(-1.44428955719596,26.5031999223435,4.26230188487573));
#6563=CARTESIAN_POINT('Ctrl Pts',(-2.82919539088272,26.6281999223435,3.79302376067927));
#6564=CARTESIAN_POINT('Ctrl Pts',(-3.67377298531816,26.7531999223436,2.59934255826103));
#6565=CARTESIAN_POINT('Ctrl Pts',(-4.5183505797536,26.8781999223435,1.40566135584279));
#6566=CARTESIAN_POINT('Ctrl Pts',(-4.5,27.0031999223436,-0.0564772772052853));
#6567=CARTESIAN_POINT('Ctrl Pts',(-4.4816494202464,27.1281999223436,-1.51861591025336));
#6568=CARTESIAN_POINT('Ctrl Pts',(-3.60737996405636,27.2531999223435,-2.69072471237123));
#6569=CARTESIAN_POINT('Ctrl Pts',(-2.73311050786633,27.3781999223436,-3.8628335144891));
#6570=CARTESIAN_POINT('Ctrl Pts',(-1.33686339217857,27.5031999223435,-4.29720676178065));
#6571=CARTESIAN_POINT('Ctrl Pts',(0.0593837235091902,27.6281999223435,-4.7315800090722));
#6572=CARTESIAN_POINT('Ctrl Pts',(1.44428955719596,27.7531999223435,-4.26230188487573));
#6573=CARTESIAN_POINT('Ctrl Pts',(2.82919539088272,27.8781999223435,-3.79302376067926));
#6574=CARTESIAN_POINT('Ctrl Pts',(3.67377298531816,28.0031999223436,-2.59934255826103));
#6575=CARTESIAN_POINT('Ctrl Pts',(4.5183505797536,28.1281999223435,-1.40566135584279));
#6576=CARTESIAN_POINT('Ctrl Pts',(4.5,28.2531999223435,0.0564772772052848));
#6577=CARTESIAN_POINT('Ctrl Pts',(4.4816494202464,28.3781999223436,1.51861591025336));
#6578=CARTESIAN_POINT('Ctrl Pts',(3.60737996405636,28.5031999223435,2.69072471237123));
#6579=CARTESIAN_POINT('Ctrl Pts',(2.73311050786633,28.6281999223435,3.8628335144891));
#6580=CARTESIAN_POINT('Ctrl Pts',(1.33686339217857,28.7531999223435,4.29720676178065));
#6581=CARTESIAN_POINT('Ctrl Pts',(-0.0593837235091896,28.8781999223435,
4.7315800090722));
#6582=CARTESIAN_POINT('Ctrl Pts',(-1.44428955719596,29.0031999223435,4.26230188487573));
#6583=CARTESIAN_POINT('Ctrl Pts',(-2.82919539088272,29.1281999223435,3.79302376067927));
#6584=CARTESIAN_POINT('Ctrl Pts',(-3.67377298531816,29.2531999223435,2.59934255826103));
#6585=CARTESIAN_POINT('Ctrl Pts',(-4.5183505797536,29.3781999223436,1.40566135584279));
#6586=CARTESIAN_POINT('Ctrl Pts',(-4.5,29.5031999223435,-0.0564772772052853));
#6587=CARTESIAN_POINT('Ctrl Pts',(-4.4816494202464,29.6281999223435,-1.51861591025336));
#6588=CARTESIAN_POINT('Ctrl Pts',(-3.60737996405636,29.7531999223435,-2.69072471237123));
#6589=CARTESIAN_POINT('Ctrl Pts',(-2.73311050786633,29.8781999223435,-3.8628335144891));
#6590=CARTESIAN_POINT('Ctrl Pts',(-1.33686339217857,30.0031999223435,-4.29720676178065));
#6591=CARTESIAN_POINT('Ctrl Pts',(0.0593837235091902,30.1281999223435,-4.7315800090722));
#6592=CARTESIAN_POINT('Ctrl Pts',(1.44428955719596,30.2531999223435,-4.26230188487573));
#6593=CARTESIAN_POINT('Ctrl Pts',(2.82919539088272,30.3781999223435,-3.79302376067926));
#6594=CARTESIAN_POINT('Ctrl Pts',(3.67377298531816,30.5031999223435,-2.59934255826103));
#6595=CARTESIAN_POINT('Ctrl Pts',(4.5183505797536,30.6281999223435,-1.40566135584279));
#6596=CARTESIAN_POINT('Ctrl Pts',(4.5,30.7531999223435,0.0564772772052848));
#6597=CARTESIAN_POINT('Ctrl Pts',(4.4816494202464,30.8781999223435,1.51861591025336));
#6598=CARTESIAN_POINT('Ctrl Pts',(3.60737996405636,31.0031999223435,2.69072471237123));
#6599=CARTESIAN_POINT('Ctrl Pts',(2.73311050786633,31.1281999223435,3.8628335144891));
#6600=CARTESIAN_POINT('Ctrl Pts',(1.33686339217857,31.2531999223435,4.29720676178065));
#6601=CARTESIAN_POINT('Ctrl Pts',(-0.0593837235091896,31.3781999223435,
4.7315800090722));
#6602=CARTESIAN_POINT('Ctrl Pts',(-1.44428955719596,31.5031999223435,4.26230188487573));
#6603=CARTESIAN_POINT('Ctrl Pts',(-2.82919539088272,31.6281999223435,3.79302376067927));
#6604=CARTESIAN_POINT('Ctrl Pts',(-3.67377298531816,31.7531999223436,2.59934255826103));
#6605=CARTESIAN_POINT('Ctrl Pts',(-4.5183505797536,31.8781999223435,1.40566135584279));
#6606=CARTESIAN_POINT('Ctrl Pts',(-4.5,32.0031999223435,-0.0564772772052853));
#6607=CARTESIAN_POINT('Ctrl Pts',(-4.4816494202464,32.1281999223435,-1.51861591025336));
#6608=CARTESIAN_POINT('Ctrl Pts',(-3.60737996405636,32.2531999223435,-2.69072471237123));
#6609=CARTESIAN_POINT('Ctrl Pts',(-2.73311050786633,32.3781999223435,-3.8628335144891));
#6610=CARTESIAN_POINT('Ctrl Pts',(-1.33686339217857,32.5031999223435,-4.29720676178065));
#6611=CARTESIAN_POINT('Ctrl Pts',(0.0593837235091902,32.6281999223435,-4.7315800090722));
#6612=CARTESIAN_POINT('Ctrl Pts',(1.44428955719596,32.7531999223435,-4.26230188487573));
#6613=CARTESIAN_POINT('Ctrl Pts',(2.82919539088272,32.8781999223435,-3.79302376067926));
#6614=CARTESIAN_POINT('Ctrl Pts',(3.67377298531816,33.0031999223436,-2.59934255826103));
#6615=CARTESIAN_POINT('Ctrl Pts',(4.5183505797536,33.1281999223435,-1.40566135584279));
#6616=CARTESIAN_POINT('Ctrl Pts',(4.5,33.2531999223435,0.0564772772052848));
#6617=CARTESIAN_POINT('Ctrl Pts',(4.4816494202464,33.3781999223435,1.51861591025336));
#6618=CARTESIAN_POINT('Ctrl Pts',(3.60737996405636,33.5031999223435,2.69072471237123));
#6619=CARTESIAN_POINT('Ctrl Pts',(2.73311050786633,33.6281999223436,3.8628335144891));
#6620=CARTESIAN_POINT('Ctrl Pts',(1.33686339217857,33.7531999223435,4.29720676178065));
#6621=CARTESIAN_POINT('Ctrl Pts',(-0.0593837235091896,33.8781999223435,
4.7315800090722));
#6622=CARTESIAN_POINT('Ctrl Pts',(-1.44428955719596,34.0031999223435,4.26230188487573));
#6623=CARTESIAN_POINT('Ctrl Pts',(-2.82919539088272,34.1281999223435,3.79302376067927));
#6624=CARTESIAN_POINT('Ctrl Pts',(-3.67377298531816,34.2531999223435,2.59934255826103));
#6625=CARTESIAN_POINT('Ctrl Pts',(-4.5183505797536,34.3781999223435,1.40566135584279));
#6626=CARTESIAN_POINT('Ctrl Pts',(-4.5,34.5031999223435,-0.0564772772052853));
#6627=CARTESIAN_POINT('Ctrl Pts',(-4.4816494202464,34.6281999223435,-1.51861591025336));
#6628=CARTESIAN_POINT('Ctrl Pts',(-3.60737996405636,34.7531999223435,-2.69072471237123));
#6629=CARTESIAN_POINT('Ctrl Pts',(-2.73311050786633,34.8781999223436,-3.8628335144891));
#6630=CARTESIAN_POINT('Ctrl Pts',(-1.33686339217857,35.0031999223435,-4.29720676178065));
#6631=CARTESIAN_POINT('Ctrl Pts',(0.0593837235091902,35.1281999223435,-4.7315800090722));
#6632=CARTESIAN_POINT('Ctrl Pts',(1.44428955719596,35.2531999223435,-4.26230188487573));
#6633=CARTESIAN_POINT('Ctrl Pts',(2.82919539088272,35.3781999223435,-3.79302376067926));
#6634=CARTESIAN_POINT('Ctrl Pts',(3.67377298531816,35.5031999223436,-2.59934255826103));
#6635=CARTESIAN_POINT('Ctrl Pts',(4.5183505797536,35.6281999223435,-1.40566135584279));
#6636=CARTESIAN_POINT('Ctrl Pts',(4.5,35.7531999223435,0.0564772772052848));
#6637=CARTESIAN_POINT('Ctrl Pts',(4.4816494202464,35.8781999223435,1.51861591025336));
#6638=CARTESIAN_POINT('Ctrl Pts',(3.60737996405636,36.0031999223435,2.69072471237123));
#6639=CARTESIAN_POINT('Ctrl Pts',(2.73311050786633,36.1281999223436,3.8628335144891));
#6640=CARTESIAN_POINT('Ctrl Pts',(1.33686339217857,36.2531999223435,4.29720676178065));
#6641=CARTESIAN_POINT('Ctrl Pts',(-0.0593837235091896,36.3781999223435,
4.7315800090722));
#6642=CARTESIAN_POINT('Ctrl Pts',(-1.44428955719596,36.5031999223435,4.26230188487573));
#6643=CARTESIAN_POINT('Ctrl Pts',(-2.82919539088272,36.6281999223435,3.79302376067927));
#6644=CARTESIAN_POINT('Ctrl Pts',(-3.67377298531816,36.7531999223435,2.59934255826103));
#6645=CARTESIAN_POINT('Ctrl Pts',(-4.5183505797536,36.8781999223435,1.40566135584279));
#6646=CARTESIAN_POINT('Ctrl Pts',(-4.5,37.0031999223435,-0.0564772772052853));
#6647=CARTESIAN_POINT('Ctrl Pts',(-4.4816494202464,37.1281999223435,-1.51861591025336));
#6648=CARTESIAN_POINT('Ctrl Pts',(-3.60737996405636,37.2531999223435,-2.69072471237123));
#6649=CARTESIAN_POINT('Ctrl Pts',(-2.73311050786633,37.3781999223436,-3.8628335144891));
#6650=CARTESIAN_POINT('Ctrl Pts',(-1.33686339217857,37.5031999223435,-4.29720676178065));
#6651=CARTESIAN_POINT('Ctrl Pts',(0.0593837235091902,37.6281999223435,-4.7315800090722));
#6652=CARTESIAN_POINT('Ctrl Pts',(1.44428955719596,37.7531999223435,-4.26230188487573));
#6653=CARTESIAN_POINT('Ctrl Pts',(2.82919539088272,37.8781999223435,-3.79302376067926));
#6654=CARTESIAN_POINT('Ctrl Pts',(3.67377298531816,38.0031999223435,-2.59934255826103));
#6655=CARTESIAN_POINT('Ctrl Pts',(4.5183505797536,38.1281999223435,-1.40566135584279));
#6656=CARTESIAN_POINT('Ctrl Pts',(4.5,38.2531999223435,0.0564772772052848));
#6657=CARTESIAN_POINT('Ctrl Pts',(4.4816494202464,38.3781999223435,1.51861591025336));
#6658=CARTESIAN_POINT('Ctrl Pts',(3.60737996405636,38.5031999223435,2.69072471237123));
#6659=CARTESIAN_POINT('Ctrl Pts',(2.73311050786633,38.6281999223436,3.8628335144891));
#6660=CARTESIAN_POINT('Ctrl Pts',(1.33686339217857,38.7531999223435,4.29720676178065));
#6661=CARTESIAN_POINT('Ctrl Pts',(-0.0593837235091896,38.8781999223435,
4.7315800090722));
#6662=CARTESIAN_POINT('Ctrl Pts',(-1.44428955719596,39.0031999223435,4.26230188487573));
#6663=CARTESIAN_POINT('Ctrl Pts',(-2.82919539088272,39.1281999223435,3.79302376067927));
#6664=CARTESIAN_POINT('Ctrl Pts',(-3.67377298531816,39.2531999223436,2.59934255826103));
#6665=CARTESIAN_POINT('Ctrl Pts',(-4.5183505797536,39.3781999223435,1.40566135584279));
#6666=CARTESIAN_POINT('Ctrl Pts',(-4.5,39.5031999223435,-0.0564772772052853));
#6667=CARTESIAN_POINT('Ctrl Pts',(-4.5,15.4968000776565,0.0564772772053793));
#6668=CARTESIAN_POINT('Ctrl Pts',(-4.51835057975363,15.6218000776565,-1.4056613558427));
#6669=CARTESIAN_POINT('Ctrl Pts',(-3.67377298531822,15.7468000776565,-2.59934255826095));
#6670=CARTESIAN_POINT('Ctrl Pts',(-2.82919539088281,15.8718000776565,-3.79302376067921));
#6671=CARTESIAN_POINT('Ctrl Pts',(-1.44428955719605,15.9968000776565,-4.2623018848757));
#6672=CARTESIAN_POINT('Ctrl Pts',(-0.0593837235092896,16.1218000776565,
-4.7315800090722));
#6673=CARTESIAN_POINT('Ctrl Pts',(1.33686339217848,16.2468000776565,-4.29720676178068));
#6674=CARTESIAN_POINT('Ctrl Pts',(2.73311050786625,16.3718000776565,-3.86283351448915));
#6675=CARTESIAN_POINT('Ctrl Pts',(3.60737996405631,16.4968000776565,-2.69072471237131));
#6676=CARTESIAN_POINT('Ctrl Pts',(4.48164942024637,16.6218000776565,-1.51861591025346));
#6677=CARTESIAN_POINT('Ctrl Pts',(4.5,16.7468000776565,-0.0564772772053798));
#6678=CARTESIAN_POINT('Ctrl Pts',(4.51835057975363,16.8718000776565,1.4056613558427));
#6679=CARTESIAN_POINT('Ctrl Pts',(3.67377298531822,16.9968000776565,2.59934255826095));
#6680=CARTESIAN_POINT('Ctrl Pts',(2.82919539088281,17.1218000776565,3.7930237606792));
#6681=CARTESIAN_POINT('Ctrl Pts',(1.44428955719605,17.2468000776565,4.2623018848757));
#6682=CARTESIAN_POINT('Ctrl Pts',(0.0593837235092902,17.3718000776565,4.7315800090722));
#6683=CARTESIAN_POINT('Ctrl Pts',(-1.33686339217848,17.4968000776565,4.29720676178068));
#6684=CARTESIAN_POINT('Ctrl Pts',(-2.73311050786625,17.6218000776565,3.86283351448915));
#6685=CARTESIAN_POINT('Ctrl Pts',(-3.60737996405631,17.7468000776565,2.69072471237131));
#6686=CARTESIAN_POINT('Ctrl Pts',(-4.48164942024637,17.8718000776565,1.51861591025346));
#6687=CARTESIAN_POINT('Ctrl Pts',(-4.5,17.9968000776565,0.0564772772053793));
#6688=CARTESIAN_POINT('Ctrl Pts',(-4.51835057975363,18.1218000776565,-1.4056613558427));
#6689=CARTESIAN_POINT('Ctrl Pts',(-3.67377298531822,18.2468000776565,-2.59934255826095));
#6690=CARTESIAN_POINT('Ctrl Pts',(-2.82919539088281,18.3718000776565,-3.79302376067921));
#6691=CARTESIAN_POINT('Ctrl Pts',(-1.44428955719605,18.4968000776565,-4.2623018848757));
#6692=CARTESIAN_POINT('Ctrl Pts',(-0.0593837235092896,18.6218000776565,
-4.7315800090722));
#6693=CARTESIAN_POINT('Ctrl Pts',(1.33686339217848,18.7468000776565,-4.29720676178068));
#6694=CARTESIAN_POINT('Ctrl Pts',(2.73311050786625,18.8718000776565,-3.86283351448915));
#6695=CARTESIAN_POINT('Ctrl Pts',(3.60737996405631,18.9968000776565,-2.69072471237131));
#6696=CARTESIAN_POINT('Ctrl Pts',(4.48164942024637,19.1218000776565,-1.51861591025346));
#6697=CARTESIAN_POINT('Ctrl Pts',(4.5,19.2468000776565,-0.0564772772053798));
#6698=CARTESIAN_POINT('Ctrl Pts',(4.51835057975363,19.3718000776565,1.4056613558427));
#6699=CARTESIAN_POINT('Ctrl Pts',(3.67377298531822,19.4968000776565,2.59934255826095));
#6700=CARTESIAN_POINT('Ctrl Pts',(2.82919539088281,19.6218000776565,3.7930237606792));
#6701=CARTESIAN_POINT('Ctrl Pts',(1.44428955719605,19.7468000776565,4.2623018848757));
#6702=CARTESIAN_POINT('Ctrl Pts',(0.0593837235092902,19.8718000776565,4.7315800090722));
#6703=CARTESIAN_POINT('Ctrl Pts',(-1.33686339217848,19.9968000776565,4.29720676178068));
#6704=CARTESIAN_POINT('Ctrl Pts',(-2.73311050786625,20.1218000776565,3.86283351448915));
#6705=CARTESIAN_POINT('Ctrl Pts',(-3.60737996405631,20.2468000776565,2.69072471237131));
#6706=CARTESIAN_POINT('Ctrl Pts',(-4.48164942024637,20.3718000776565,1.51861591025346));
#6707=CARTESIAN_POINT('Ctrl Pts',(-4.5,20.4968000776565,0.0564772772053793));
#6708=CARTESIAN_POINT('Ctrl Pts',(-4.51835057975363,20.6218000776565,-1.4056613558427));
#6709=CARTESIAN_POINT('Ctrl Pts',(-3.67377298531822,20.7468000776565,-2.59934255826095));
#6710=CARTESIAN_POINT('Ctrl Pts',(-2.82919539088281,20.8718000776565,-3.79302376067921));
#6711=CARTESIAN_POINT('Ctrl Pts',(-1.44428955719605,20.9968000776565,-4.2623018848757));
#6712=CARTESIAN_POINT('Ctrl Pts',(-0.0593837235092896,21.1218000776565,
-4.7315800090722));
#6713=CARTESIAN_POINT('Ctrl Pts',(1.33686339217848,21.2468000776565,-4.29720676178068));
#6714=CARTESIAN_POINT('Ctrl Pts',(2.73311050786625,21.3718000776565,-3.86283351448915));
#6715=CARTESIAN_POINT('Ctrl Pts',(3.60737996405631,21.4968000776565,-2.69072471237131));
#6716=CARTESIAN_POINT('Ctrl Pts',(4.48164942024637,21.6218000776565,-1.51861591025346));
#6717=CARTESIAN_POINT('Ctrl Pts',(4.5,21.7468000776565,-0.0564772772053798));
#6718=CARTESIAN_POINT('Ctrl Pts',(4.51835057975363,21.8718000776565,1.4056613558427));
#6719=CARTESIAN_POINT('Ctrl Pts',(3.67377298531822,21.9968000776565,2.59934255826095));
#6720=CARTESIAN_POINT('Ctrl Pts',(2.82919539088281,22.1218000776565,3.7930237606792));
#6721=CARTESIAN_POINT('Ctrl Pts',(1.44428955719605,22.2468000776565,4.2623018848757));
#6722=CARTESIAN_POINT('Ctrl Pts',(0.0593837235092902,22.3718000776565,4.7315800090722));
#6723=CARTESIAN_POINT('Ctrl Pts',(-1.33686339217848,22.4968000776565,4.29720676178068));
#6724=CARTESIAN_POINT('Ctrl Pts',(-2.73311050786625,22.6218000776565,3.86283351448915));
#6725=CARTESIAN_POINT('Ctrl Pts',(-3.60737996405631,22.7468000776565,2.69072471237131));
#6726=CARTESIAN_POINT('Ctrl Pts',(-4.48164942024637,22.8718000776565,1.51861591025346));
#6727=CARTESIAN_POINT('Ctrl Pts',(-4.5,22.9968000776565,0.0564772772053793));
#6728=CARTESIAN_POINT('Ctrl Pts',(-4.51835057975363,23.1218000776565,-1.4056613558427));
#6729=CARTESIAN_POINT('Ctrl Pts',(-3.67377298531822,23.2468000776565,-2.59934255826095));
#6730=CARTESIAN_POINT('Ctrl Pts',(-2.82919539088281,23.3718000776565,-3.79302376067921));
#6731=CARTESIAN_POINT('Ctrl Pts',(-1.44428955719605,23.4968000776565,-4.2623018848757));
#6732=CARTESIAN_POINT('Ctrl Pts',(-0.0593837235092896,23.6218000776565,
-4.7315800090722));
#6733=CARTESIAN_POINT('Ctrl Pts',(1.33686339217848,23.7468000776565,-4.29720676178068));
#6734=CARTESIAN_POINT('Ctrl Pts',(2.73311050786625,23.8718000776565,-3.86283351448915));
#6735=CARTESIAN_POINT('Ctrl Pts',(3.60737996405631,23.9968000776565,-2.69072471237131));
#6736=CARTESIAN_POINT('Ctrl Pts',(4.48164942024637,24.1218000776565,-1.51861591025346));
#6737=CARTESIAN_POINT('Ctrl Pts',(4.5,24.2468000776565,-0.0564772772053798));
#6738=CARTESIAN_POINT('Ctrl Pts',(4.51835057975363,24.3718000776565,1.4056613558427));
#6739=CARTESIAN_POINT('Ctrl Pts',(3.67377298531822,24.4968000776565,2.59934255826095));
#6740=CARTESIAN_POINT('Ctrl Pts',(2.82919539088281,24.6218000776565,3.7930237606792));
#6741=CARTESIAN_POINT('Ctrl Pts',(1.44428955719605,24.7468000776565,4.2623018848757));
#6742=CARTESIAN_POINT('Ctrl Pts',(0.0593837235092902,24.8718000776565,4.7315800090722));
#6743=CARTESIAN_POINT('Ctrl Pts',(-1.33686339217848,24.9968000776565,4.29720676178068));
#6744=CARTESIAN_POINT('Ctrl Pts',(-2.73311050786625,25.1218000776565,3.86283351448915));
#6745=CARTESIAN_POINT('Ctrl Pts',(-3.60737996405631,25.2468000776565,2.69072471237131));
#6746=CARTESIAN_POINT('Ctrl Pts',(-4.48164942024637,25.3718000776565,1.51861591025346));
#6747=CARTESIAN_POINT('Ctrl Pts',(-4.5,25.4968000776565,0.0564772772053793));
#6748=CARTESIAN_POINT('Ctrl Pts',(-4.51835057975363,25.6218000776565,-1.4056613558427));
#6749=CARTESIAN_POINT('Ctrl Pts',(-3.67377298531822,25.7468000776565,-2.59934255826095));
#6750=CARTESIAN_POINT('Ctrl Pts',(-2.82919539088281,25.8718000776565,-3.79302376067921));
#6751=CARTESIAN_POINT('Ctrl Pts',(-1.44428955719605,25.9968000776565,-4.2623018848757));
#6752=CARTESIAN_POINT('Ctrl Pts',(-0.0593837235092896,26.1218000776565,
-4.7315800090722));
#6753=CARTESIAN_POINT('Ctrl Pts',(1.33686339217848,26.2468000776565,-4.29720676178068));
#6754=CARTESIAN_POINT('Ctrl Pts',(2.73311050786625,26.3718000776565,-3.86283351448915));
#6755=CARTESIAN_POINT('Ctrl Pts',(3.60737996405631,26.4968000776565,-2.69072471237131));
#6756=CARTESIAN_POINT('Ctrl Pts',(4.48164942024637,26.6218000776565,-1.51861591025346));
#6757=CARTESIAN_POINT('Ctrl Pts',(4.5,26.7468000776565,-0.0564772772053798));
#6758=CARTESIAN_POINT('Ctrl Pts',(4.51835057975363,26.8718000776565,1.4056613558427));
#6759=CARTESIAN_POINT('Ctrl Pts',(3.67377298531822,26.9968000776565,2.59934255826095));
#6760=CARTESIAN_POINT('Ctrl Pts',(2.82919539088281,27.1218000776565,3.7930237606792));
#6761=CARTESIAN_POINT('Ctrl Pts',(1.44428955719605,27.2468000776565,4.2623018848757));
#6762=CARTESIAN_POINT('Ctrl Pts',(0.0593837235092902,27.3718000776565,4.7315800090722));
#6763=CARTESIAN_POINT('Ctrl Pts',(-1.33686339217848,27.4968000776565,4.29720676178068));
#6764=CARTESIAN_POINT('Ctrl Pts',(-2.73311050786625,27.6218000776565,3.86283351448915));
#6765=CARTESIAN_POINT('Ctrl Pts',(-3.60737996405631,27.7468000776565,2.69072471237131));
#6766=CARTESIAN_POINT('Ctrl Pts',(-4.48164942024637,27.8718000776565,1.51861591025346));
#6767=CARTESIAN_POINT('Ctrl Pts',(-4.5,27.9968000776565,0.0564772772053793));
#6768=CARTESIAN_POINT('Ctrl Pts',(-4.51835057975363,28.1218000776565,-1.4056613558427));
#6769=CARTESIAN_POINT('Ctrl Pts',(-3.67377298531822,28.2468000776565,-2.59934255826095));
#6770=CARTESIAN_POINT('Ctrl Pts',(-2.82919539088281,28.3718000776565,-3.79302376067921));
#6771=CARTESIAN_POINT('Ctrl Pts',(-1.44428955719605,28.4968000776565,-4.2623018848757));
#6772=CARTESIAN_POINT('Ctrl Pts',(-0.0593837235092896,28.6218000776565,
-4.7315800090722));
#6773=CARTESIAN_POINT('Ctrl Pts',(1.33686339217848,28.7468000776565,-4.29720676178068));
#6774=CARTESIAN_POINT('Ctrl Pts',(2.73311050786625,28.8718000776565,-3.86283351448915));
#6775=CARTESIAN_POINT('Ctrl Pts',(3.60737996405631,28.9968000776565,-2.69072471237131));
#6776=CARTESIAN_POINT('Ctrl Pts',(4.48164942024637,29.1218000776565,-1.51861591025346));
#6777=CARTESIAN_POINT('Ctrl Pts',(4.5,29.2468000776565,-0.0564772772053798));
#6778=CARTESIAN_POINT('Ctrl Pts',(4.51835057975363,29.3718000776565,1.4056613558427));
#6779=CARTESIAN_POINT('Ctrl Pts',(3.67377298531822,29.4968000776565,2.59934255826095));
#6780=CARTESIAN_POINT('Ctrl Pts',(2.82919539088281,29.6218000776565,3.7930237606792));
#6781=CARTESIAN_POINT('Ctrl Pts',(1.44428955719605,29.7468000776565,4.2623018848757));
#6782=CARTESIAN_POINT('Ctrl Pts',(0.0593837235092902,29.8718000776565,4.7315800090722));
#6783=CARTESIAN_POINT('Ctrl Pts',(-1.33686339217848,29.9968000776565,4.29720676178068));
#6784=CARTESIAN_POINT('Ctrl Pts',(-2.73311050786625,30.1218000776565,3.86283351448915));
#6785=CARTESIAN_POINT('Ctrl Pts',(-3.60737996405631,30.2468000776565,2.69072471237131));
#6786=CARTESIAN_POINT('Ctrl Pts',(-4.48164942024637,30.3718000776565,1.51861591025346));
#6787=CARTESIAN_POINT('Ctrl Pts',(-4.5,30.4968000776565,0.0564772772053793));
#6788=CARTESIAN_POINT('Ctrl Pts',(-4.51835057975363,30.6218000776565,-1.4056613558427));
#6789=CARTESIAN_POINT('Ctrl Pts',(-3.67377298531822,30.7468000776565,-2.59934255826095));
#6790=CARTESIAN_POINT('Ctrl Pts',(-2.82919539088281,30.8718000776565,-3.79302376067921));
#6791=CARTESIAN_POINT('Ctrl Pts',(-1.44428955719605,30.9968000776565,-4.2623018848757));
#6792=CARTESIAN_POINT('Ctrl Pts',(-0.0593837235092896,31.1218000776565,
-4.7315800090722));
#6793=CARTESIAN_POINT('Ctrl Pts',(1.33686339217848,31.2468000776565,-4.29720676178068));
#6794=CARTESIAN_POINT('Ctrl Pts',(2.73311050786625,31.3718000776565,-3.86283351448915));
#6795=CARTESIAN_POINT('Ctrl Pts',(3.60737996405631,31.4968000776565,-2.69072471237131));
#6796=CARTESIAN_POINT('Ctrl Pts',(4.48164942024637,31.6218000776565,-1.51861591025346));
#6797=CARTESIAN_POINT('Ctrl Pts',(4.5,31.7468000776565,-0.0564772772053798));
#6798=CARTESIAN_POINT('Ctrl Pts',(4.51835057975363,31.8718000776565,1.4056613558427));
#6799=CARTESIAN_POINT('Ctrl Pts',(3.67377298531822,31.9968000776565,2.59934255826095));
#6800=CARTESIAN_POINT('Ctrl Pts',(2.82919539088281,32.1218000776565,3.7930237606792));
#6801=CARTESIAN_POINT('Ctrl Pts',(1.44428955719605,32.2468000776565,4.2623018848757));
#6802=CARTESIAN_POINT('Ctrl Pts',(0.0593837235092902,32.3718000776565,4.7315800090722));
#6803=CARTESIAN_POINT('Ctrl Pts',(-1.33686339217848,32.4968000776565,4.29720676178068));
#6804=CARTESIAN_POINT('Ctrl Pts',(-2.73311050786625,32.6218000776565,3.86283351448915));
#6805=CARTESIAN_POINT('Ctrl Pts',(-3.60737996405631,32.7468000776565,2.69072471237131));
#6806=CARTESIAN_POINT('Ctrl Pts',(-4.48164942024637,32.8718000776565,1.51861591025346));
#6807=CARTESIAN_POINT('Ctrl Pts',(-4.5,32.9968000776565,0.0564772772053793));
#6808=CARTESIAN_POINT('Ctrl Pts',(-4.51835057975363,33.1218000776565,-1.4056613558427));
#6809=CARTESIAN_POINT('Ctrl Pts',(-3.67377298531822,33.2468000776565,-2.59934255826095));
#6810=CARTESIAN_POINT('Ctrl Pts',(-2.82919539088281,33.3718000776565,-3.79302376067921));
#6811=CARTESIAN_POINT('Ctrl Pts',(-1.44428955719605,33.4968000776565,-4.2623018848757));
#6812=CARTESIAN_POINT('Ctrl Pts',(-0.0593837235092896,33.6218000776565,
-4.7315800090722));
#6813=CARTESIAN_POINT('Ctrl Pts',(1.33686339217848,33.7468000776565,-4.29720676178068));
#6814=CARTESIAN_POINT('Ctrl Pts',(2.73311050786625,33.8718000776565,-3.86283351448915));
#6815=CARTESIAN_POINT('Ctrl Pts',(3.60737996405631,33.9968000776565,-2.69072471237131));
#6816=CARTESIAN_POINT('Ctrl Pts',(4.48164942024637,34.1218000776565,-1.51861591025346));
#6817=CARTESIAN_POINT('Ctrl Pts',(4.5,34.2468000776565,-0.0564772772053798));
#6818=CARTESIAN_POINT('Ctrl Pts',(4.51835057975363,34.3718000776565,1.4056613558427));
#6819=CARTESIAN_POINT('Ctrl Pts',(3.67377298531822,34.4968000776565,2.59934255826095));
#6820=CARTESIAN_POINT('Ctrl Pts',(2.82919539088281,34.6218000776565,3.7930237606792));
#6821=CARTESIAN_POINT('Ctrl Pts',(1.44428955719605,34.7468000776565,4.2623018848757));
#6822=CARTESIAN_POINT('Ctrl Pts',(0.0593837235092902,34.8718000776565,4.7315800090722));
#6823=CARTESIAN_POINT('Ctrl Pts',(-1.33686339217848,34.9968000776565,4.29720676178068));
#6824=CARTESIAN_POINT('Ctrl Pts',(-2.73311050786625,35.1218000776565,3.86283351448915));
#6825=CARTESIAN_POINT('Ctrl Pts',(-3.60737996405631,35.2468000776565,2.69072471237131));
#6826=CARTESIAN_POINT('Ctrl Pts',(-4.48164942024637,35.3718000776565,1.51861591025346));
#6827=CARTESIAN_POINT('Ctrl Pts',(-4.5,35.4968000776565,0.0564772772053793));
#6828=CARTESIAN_POINT('Ctrl Pts',(-4.51835057975363,35.6218000776565,-1.4056613558427));
#6829=CARTESIAN_POINT('Ctrl Pts',(-3.67377298531822,35.7468000776565,-2.59934255826095));
#6830=CARTESIAN_POINT('Ctrl Pts',(-2.82919539088281,35.8718000776565,-3.79302376067921));
#6831=CARTESIAN_POINT('Ctrl Pts',(-1.44428955719605,35.9968000776565,-4.2623018848757));
#6832=CARTESIAN_POINT('Ctrl Pts',(-0.0593837235092896,36.1218000776565,
-4.7315800090722));
#6833=CARTESIAN_POINT('Ctrl Pts',(1.33686339217848,36.2468000776565,-4.29720676178068));
#6834=CARTESIAN_POINT('Ctrl Pts',(2.73311050786625,36.3718000776565,-3.86283351448915));
#6835=CARTESIAN_POINT('Ctrl Pts',(3.60737996405631,36.4968000776565,-2.69072471237131));
#6836=CARTESIAN_POINT('Ctrl Pts',(4.48164942024637,36.6218000776565,-1.51861591025346));
#6837=CARTESIAN_POINT('Ctrl Pts',(4.5,36.7468000776565,-0.0564772772053798));
#6838=CARTESIAN_POINT('Ctrl Pts',(4.51835057975363,36.8718000776565,1.4056613558427));
#6839=CARTESIAN_POINT('Ctrl Pts',(3.67377298531822,36.9968000776565,2.59934255826095));
#6840=CARTESIAN_POINT('Ctrl Pts',(2.82919539088281,37.1218000776565,3.7930237606792));
#6841=CARTESIAN_POINT('Ctrl Pts',(1.44428955719605,37.2468000776565,4.2623018848757));
#6842=CARTESIAN_POINT('Ctrl Pts',(0.0593837235092902,37.3718000776565,4.7315800090722));
#6843=CARTESIAN_POINT('Ctrl Pts',(-1.33686339217848,37.4968000776565,4.29720676178068));
#6844=CARTESIAN_POINT('Ctrl Pts',(-2.73311050786625,37.6218000776565,3.86283351448915));
#6845=CARTESIAN_POINT('Ctrl Pts',(-3.60737996405631,37.7468000776565,2.69072471237131));
#6846=CARTESIAN_POINT('Ctrl Pts',(-4.48164942024637,37.8718000776565,1.51861591025346));
#6847=CARTESIAN_POINT('Ctrl Pts',(-4.5,37.9968000776565,0.0564772772053793));
#6848=CARTESIAN_POINT('Ctrl Pts',(-4.51835057975363,38.1218000776565,-1.4056613558427));
#6849=CARTESIAN_POINT('Ctrl Pts',(-3.67377298531822,38.2468000776565,-2.59934255826095));
#6850=CARTESIAN_POINT('Ctrl Pts',(-2.82919539088281,38.3718000776565,-3.79302376067921));
#6851=CARTESIAN_POINT('Ctrl Pts',(-1.44428955719605,38.4968000776565,-4.2623018848757));
#6852=CARTESIAN_POINT('Ctrl Pts',(-0.0593837235092896,38.6218000776565,
-4.7315800090722));
#6853=CARTESIAN_POINT('Ctrl Pts',(1.33686339217848,38.7468000776565,-4.29720676178068));
#6854=CARTESIAN_POINT('Ctrl Pts',(2.73311050786625,38.8718000776565,-3.86283351448915));
#6855=CARTESIAN_POINT('Ctrl Pts',(3.60737996405631,38.9968000776565,-2.69072471237131));
#6856=CARTESIAN_POINT('Ctrl Pts',(4.48164942024637,39.1218000776565,-1.51861591025346));
#6857=CARTESIAN_POINT('Ctrl Pts',(4.5,39.2468000776565,-0.0564772772053798));
#6858=CARTESIAN_POINT('Ctrl Pts',(4.51835057975363,39.3718000776565,1.4056613558427));
#6859=CARTESIAN_POINT('Ctrl Pts',(3.67377298531822,39.4968000776565,2.59934255826095));
#6860=CARTESIAN_POINT('Ctrl Pts',(2.82919539088281,39.6218000776565,3.7930237606792));
#6861=CARTESIAN_POINT('Ctrl Pts',(1.44428955719605,39.7468000776565,4.2623018848757));
#6862=CARTESIAN_POINT('Ctrl Pts',(0.0593837235092902,39.8718000776565,4.7315800090722));
#6863=CARTESIAN_POINT('Ctrl Pts',(-1.33686339217848,39.9968000776565,4.29720676178068));
#6864=CARTESIAN_POINT('Ctrl Pts',(-2.73311050786625,40.1218000776565,3.86283351448915));
#6865=CARTESIAN_POINT('Ctrl Pts',(-3.60737996405631,40.2468000776565,2.69072471237131));
#6866=CARTESIAN_POINT('Ctrl Pts',(-4.48164942024637,40.3718000776565,1.51861591025346));
#6867=CARTESIAN_POINT('Ctrl Pts',(-4.5,40.4968000776565,0.0564772772053793));
#6868=CARTESIAN_POINT('Ctrl Pts',(-3.5,15.4968000776565,0.0564772772053689));
#6869=CARTESIAN_POINT('Ctrl Pts',(-3.51835057975363,15.6218000776565,-1.0807416596098));
#6870=CARTESIAN_POINT('Ctrl Pts',(-2.86475599094327,15.7468000776565,-2.01155730596849));
#6871=CARTESIAN_POINT('Ctrl Pts',(-2.2111614021329,15.8718000776565,-2.94237295232717));
#6872=CARTESIAN_POINT('Ctrl Pts',(-1.13527256282109,15.9968000776565,-3.31124536858055));
#6873=CARTESIAN_POINT('Ctrl Pts',(-0.0593837235092786,16.1218000776565,
-3.68011778483394));
#6874=CARTESIAN_POINT('Ctrl Pts',(1.02784639780354,16.2468000776565,-3.34615024548552));
#6875=CARTESIAN_POINT('Ctrl Pts',(2.11507651911636,16.3718000776565,-3.01218270613711));
#6876=CARTESIAN_POINT('Ctrl Pts',(2.79836296968137,16.4968000776565,-2.10293946007882));
#6877=CARTESIAN_POINT('Ctrl Pts',(3.48164942024637,16.6218000776565,-1.19369621402054));
#6878=CARTESIAN_POINT('Ctrl Pts',(3.5,16.7468000776565,-0.0564772772053694));
#6879=CARTESIAN_POINT('Ctrl Pts',(3.51835057975363,16.8718000776565,1.0807416596098));
#6880=CARTESIAN_POINT('Ctrl Pts',(2.86475599094327,16.9968000776565,2.01155730596849));
#6881=CARTESIAN_POINT('Ctrl Pts',(2.2111614021329,17.1218000776565,2.94237295232717));
#6882=CARTESIAN_POINT('Ctrl Pts',(1.13527256282109,17.2468000776565,3.31124536858055));
#6883=CARTESIAN_POINT('Ctrl Pts',(0.0593837235092791,17.3718000776565,3.68011778483394));
#6884=CARTESIAN_POINT('Ctrl Pts',(-1.02784639780354,17.4968000776565,3.34615024548552));
#6885=CARTESIAN_POINT('Ctrl Pts',(-2.11507651911636,17.6218000776565,3.01218270613711));
#6886=CARTESIAN_POINT('Ctrl Pts',(-2.79836296968137,17.7468000776565,2.10293946007882));
#6887=CARTESIAN_POINT('Ctrl Pts',(-3.48164942024637,17.8718000776565,1.19369621402054));
#6888=CARTESIAN_POINT('Ctrl Pts',(-3.5,17.9968000776565,0.0564772772053689));
#6889=CARTESIAN_POINT('Ctrl Pts',(-3.51835057975363,18.1218000776565,-1.0807416596098));
#6890=CARTESIAN_POINT('Ctrl Pts',(-2.86475599094327,18.2468000776565,-2.01155730596849));
#6891=CARTESIAN_POINT('Ctrl Pts',(-2.2111614021329,18.3718000776565,-2.94237295232717));
#6892=CARTESIAN_POINT('Ctrl Pts',(-1.13527256282109,18.4968000776565,-3.31124536858055));
#6893=CARTESIAN_POINT('Ctrl Pts',(-0.0593837235092786,18.6218000776565,
-3.68011778483394));
#6894=CARTESIAN_POINT('Ctrl Pts',(1.02784639780354,18.7468000776565,-3.34615024548552));
#6895=CARTESIAN_POINT('Ctrl Pts',(2.11507651911636,18.8718000776565,-3.01218270613711));
#6896=CARTESIAN_POINT('Ctrl Pts',(2.79836296968137,18.9968000776565,-2.10293946007882));
#6897=CARTESIAN_POINT('Ctrl Pts',(3.48164942024637,19.1218000776565,-1.19369621402054));
#6898=CARTESIAN_POINT('Ctrl Pts',(3.5,19.2468000776565,-0.0564772772053694));
#6899=CARTESIAN_POINT('Ctrl Pts',(3.51835057975363,19.3718000776565,1.0807416596098));
#6900=CARTESIAN_POINT('Ctrl Pts',(2.86475599094327,19.4968000776565,2.01155730596849));
#6901=CARTESIAN_POINT('Ctrl Pts',(2.2111614021329,19.6218000776565,2.94237295232717));
#6902=CARTESIAN_POINT('Ctrl Pts',(1.13527256282109,19.7468000776565,3.31124536858055));
#6903=CARTESIAN_POINT('Ctrl Pts',(0.0593837235092791,19.8718000776565,3.68011778483394));
#6904=CARTESIAN_POINT('Ctrl Pts',(-1.02784639780354,19.9968000776565,3.34615024548552));
#6905=CARTESIAN_POINT('Ctrl Pts',(-2.11507651911636,20.1218000776565,3.01218270613711));
#6906=CARTESIAN_POINT('Ctrl Pts',(-2.79836296968137,20.2468000776565,2.10293946007882));
#6907=CARTESIAN_POINT('Ctrl Pts',(-3.48164942024637,20.3718000776565,1.19369621402054));
#6908=CARTESIAN_POINT('Ctrl Pts',(-3.5,20.4968000776565,0.0564772772053689));
#6909=CARTESIAN_POINT('Ctrl Pts',(-3.51835057975363,20.6218000776565,-1.0807416596098));
#6910=CARTESIAN_POINT('Ctrl Pts',(-2.86475599094327,20.7468000776565,-2.01155730596849));
#6911=CARTESIAN_POINT('Ctrl Pts',(-2.2111614021329,20.8718000776565,-2.94237295232717));
#6912=CARTESIAN_POINT('Ctrl Pts',(-1.13527256282109,20.9968000776565,-3.31124536858055));
#6913=CARTESIAN_POINT('Ctrl Pts',(-0.0593837235092786,21.1218000776565,
-3.68011778483394));
#6914=CARTESIAN_POINT('Ctrl Pts',(1.02784639780354,21.2468000776565,-3.34615024548552));
#6915=CARTESIAN_POINT('Ctrl Pts',(2.11507651911636,21.3718000776565,-3.01218270613711));
#6916=CARTESIAN_POINT('Ctrl Pts',(2.79836296968137,21.4968000776565,-2.10293946007882));
#6917=CARTESIAN_POINT('Ctrl Pts',(3.48164942024637,21.6218000776565,-1.19369621402054));
#6918=CARTESIAN_POINT('Ctrl Pts',(3.5,21.7468000776565,-0.0564772772053694));
#6919=CARTESIAN_POINT('Ctrl Pts',(3.51835057975363,21.8718000776565,1.0807416596098));
#6920=CARTESIAN_POINT('Ctrl Pts',(2.86475599094327,21.9968000776565,2.01155730596849));
#6921=CARTESIAN_POINT('Ctrl Pts',(2.2111614021329,22.1218000776565,2.94237295232717));
#6922=CARTESIAN_POINT('Ctrl Pts',(1.13527256282109,22.2468000776565,3.31124536858055));
#6923=CARTESIAN_POINT('Ctrl Pts',(0.0593837235092791,22.3718000776565,3.68011778483394));
#6924=CARTESIAN_POINT('Ctrl Pts',(-1.02784639780354,22.4968000776565,3.34615024548552));
#6925=CARTESIAN_POINT('Ctrl Pts',(-2.11507651911636,22.6218000776565,3.01218270613711));
#6926=CARTESIAN_POINT('Ctrl Pts',(-2.79836296968137,22.7468000776565,2.10293946007882));
#6927=CARTESIAN_POINT('Ctrl Pts',(-3.48164942024637,22.8718000776565,1.19369621402054));
#6928=CARTESIAN_POINT('Ctrl Pts',(-3.5,22.9968000776565,0.0564772772053689));
#6929=CARTESIAN_POINT('Ctrl Pts',(-3.51835057975363,23.1218000776565,-1.0807416596098));
#6930=CARTESIAN_POINT('Ctrl Pts',(-2.86475599094327,23.2468000776565,-2.01155730596849));
#6931=CARTESIAN_POINT('Ctrl Pts',(-2.2111614021329,23.3718000776565,-2.94237295232717));
#6932=CARTESIAN_POINT('Ctrl Pts',(-1.13527256282109,23.4968000776565,-3.31124536858055));
#6933=CARTESIAN_POINT('Ctrl Pts',(-0.0593837235092786,23.6218000776565,
-3.68011778483394));
#6934=CARTESIAN_POINT('Ctrl Pts',(1.02784639780354,23.7468000776565,-3.34615024548552));
#6935=CARTESIAN_POINT('Ctrl Pts',(2.11507651911636,23.8718000776565,-3.01218270613711));
#6936=CARTESIAN_POINT('Ctrl Pts',(2.79836296968137,23.9968000776565,-2.10293946007882));
#6937=CARTESIAN_POINT('Ctrl Pts',(3.48164942024637,24.1218000776565,-1.19369621402054));
#6938=CARTESIAN_POINT('Ctrl Pts',(3.5,24.2468000776565,-0.0564772772053694));
#6939=CARTESIAN_POINT('Ctrl Pts',(3.51835057975363,24.3718000776565,1.0807416596098));
#6940=CARTESIAN_POINT('Ctrl Pts',(2.86475599094327,24.4968000776565,2.01155730596849));
#6941=CARTESIAN_POINT('Ctrl Pts',(2.2111614021329,24.6218000776565,2.94237295232717));
#6942=CARTESIAN_POINT('Ctrl Pts',(1.13527256282109,24.7468000776565,3.31124536858055));
#6943=CARTESIAN_POINT('Ctrl Pts',(0.0593837235092791,24.8718000776565,3.68011778483394));
#6944=CARTESIAN_POINT('Ctrl Pts',(-1.02784639780354,24.9968000776565,3.34615024548552));
#6945=CARTESIAN_POINT('Ctrl Pts',(-2.11507651911636,25.1218000776565,3.01218270613711));
#6946=CARTESIAN_POINT('Ctrl Pts',(-2.79836296968137,25.2468000776565,2.10293946007882));
#6947=CARTESIAN_POINT('Ctrl Pts',(-3.48164942024637,25.3718000776565,1.19369621402054));
#6948=CARTESIAN_POINT('Ctrl Pts',(-3.5,25.4968000776565,0.0564772772053689));
#6949=CARTESIAN_POINT('Ctrl Pts',(-3.51835057975363,25.6218000776565,-1.0807416596098));
#6950=CARTESIAN_POINT('Ctrl Pts',(-2.86475599094327,25.7468000776565,-2.01155730596849));
#6951=CARTESIAN_POINT('Ctrl Pts',(-2.2111614021329,25.8718000776565,-2.94237295232717));
#6952=CARTESIAN_POINT('Ctrl Pts',(-1.13527256282109,25.9968000776565,-3.31124536858055));
#6953=CARTESIAN_POINT('Ctrl Pts',(-0.0593837235092786,26.1218000776565,
-3.68011778483394));
#6954=CARTESIAN_POINT('Ctrl Pts',(1.02784639780354,26.2468000776565,-3.34615024548552));
#6955=CARTESIAN_POINT('Ctrl Pts',(2.11507651911636,26.3718000776565,-3.01218270613711));
#6956=CARTESIAN_POINT('Ctrl Pts',(2.79836296968137,26.4968000776565,-2.10293946007882));
#6957=CARTESIAN_POINT('Ctrl Pts',(3.48164942024637,26.6218000776565,-1.19369621402054));
#6958=CARTESIAN_POINT('Ctrl Pts',(3.5,26.7468000776565,-0.0564772772053694));
#6959=CARTESIAN_POINT('Ctrl Pts',(3.51835057975363,26.8718000776565,1.0807416596098));
#6960=CARTESIAN_POINT('Ctrl Pts',(2.86475599094327,26.9968000776565,2.01155730596849));
#6961=CARTESIAN_POINT('Ctrl Pts',(2.2111614021329,27.1218000776565,2.94237295232717));
#6962=CARTESIAN_POINT('Ctrl Pts',(1.13527256282109,27.2468000776565,3.31124536858055));
#6963=CARTESIAN_POINT('Ctrl Pts',(0.0593837235092791,27.3718000776565,3.68011778483394));
#6964=CARTESIAN_POINT('Ctrl Pts',(-1.02784639780354,27.4968000776565,3.34615024548552));
#6965=CARTESIAN_POINT('Ctrl Pts',(-2.11507651911636,27.6218000776565,3.01218270613711));
#6966=CARTESIAN_POINT('Ctrl Pts',(-2.79836296968137,27.7468000776565,2.10293946007882));
#6967=CARTESIAN_POINT('Ctrl Pts',(-3.48164942024637,27.8718000776565,1.19369621402054));
#6968=CARTESIAN_POINT('Ctrl Pts',(-3.5,27.9968000776565,0.0564772772053689));
#6969=CARTESIAN_POINT('Ctrl Pts',(-3.51835057975363,28.1218000776565,-1.0807416596098));
#6970=CARTESIAN_POINT('Ctrl Pts',(-2.86475599094327,28.2468000776565,-2.01155730596849));
#6971=CARTESIAN_POINT('Ctrl Pts',(-2.2111614021329,28.3718000776565,-2.94237295232717));
#6972=CARTESIAN_POINT('Ctrl Pts',(-1.13527256282109,28.4968000776565,-3.31124536858055));
#6973=CARTESIAN_POINT('Ctrl Pts',(-0.0593837235092786,28.6218000776565,
-3.68011778483394));
#6974=CARTESIAN_POINT('Ctrl Pts',(1.02784639780354,28.7468000776565,-3.34615024548552));
#6975=CARTESIAN_POINT('Ctrl Pts',(2.11507651911636,28.8718000776565,-3.01218270613711));
#6976=CARTESIAN_POINT('Ctrl Pts',(2.79836296968137,28.9968000776565,-2.10293946007882));
#6977=CARTESIAN_POINT('Ctrl Pts',(3.48164942024637,29.1218000776565,-1.19369621402054));
#6978=CARTESIAN_POINT('Ctrl Pts',(3.5,29.2468000776565,-0.0564772772053694));
#6979=CARTESIAN_POINT('Ctrl Pts',(3.51835057975363,29.3718000776565,1.0807416596098));
#6980=CARTESIAN_POINT('Ctrl Pts',(2.86475599094327,29.4968000776565,2.01155730596849));
#6981=CARTESIAN_POINT('Ctrl Pts',(2.2111614021329,29.6218000776565,2.94237295232717));
#6982=CARTESIAN_POINT('Ctrl Pts',(1.13527256282109,29.7468000776565,3.31124536858055));
#6983=CARTESIAN_POINT('Ctrl Pts',(0.0593837235092791,29.8718000776565,3.68011778483394));
#6984=CARTESIAN_POINT('Ctrl Pts',(-1.02784639780354,29.9968000776565,3.34615024548552));
#6985=CARTESIAN_POINT('Ctrl Pts',(-2.11507651911636,30.1218000776565,3.01218270613711));
#6986=CARTESIAN_POINT('Ctrl Pts',(-2.79836296968137,30.2468000776565,2.10293946007882));
#6987=CARTESIAN_POINT('Ctrl Pts',(-3.48164942024637,30.3718000776565,1.19369621402054));
#6988=CARTESIAN_POINT('Ctrl Pts',(-3.5,30.4968000776565,0.0564772772053689));
#6989=CARTESIAN_POINT('Ctrl Pts',(-3.51835057975363,30.6218000776565,-1.0807416596098));
#6990=CARTESIAN_POINT('Ctrl Pts',(-2.86475599094327,30.7468000776565,-2.01155730596849));
#6991=CARTESIAN_POINT('Ctrl Pts',(-2.2111614021329,30.8718000776565,-2.94237295232717));
#6992=CARTESIAN_POINT('Ctrl Pts',(-1.13527256282109,30.9968000776565,-3.31124536858055));
#6993=CARTESIAN_POINT('Ctrl Pts',(-0.0593837235092786,31.1218000776565,
-3.68011778483394));
#6994=CARTESIAN_POINT('Ctrl Pts',(1.02784639780354,31.2468000776565,-3.34615024548552));
#6995=CARTESIAN_POINT('Ctrl Pts',(2.11507651911636,31.3718000776565,-3.01218270613711));
#6996=CARTESIAN_POINT('Ctrl Pts',(2.79836296968137,31.4968000776565,-2.10293946007882));
#6997=CARTESIAN_POINT('Ctrl Pts',(3.48164942024637,31.6218000776565,-1.19369621402054));
#6998=CARTESIAN_POINT('Ctrl Pts',(3.5,31.7468000776565,-0.0564772772053694));
#6999=CARTESIAN_POINT('Ctrl Pts',(3.51835057975363,31.8718000776565,1.0807416596098));
#7000=CARTESIAN_POINT('Ctrl Pts',(2.86475599094327,31.9968000776565,2.01155730596849));
#7001=CARTESIAN_POINT('Ctrl Pts',(2.2111614021329,32.1218000776565,2.94237295232717));
#7002=CARTESIAN_POINT('Ctrl Pts',(1.13527256282109,32.2468000776565,3.31124536858055));
#7003=CARTESIAN_POINT('Ctrl Pts',(0.0593837235092791,32.3718000776565,3.68011778483394));
#7004=CARTESIAN_POINT('Ctrl Pts',(-1.02784639780354,32.4968000776565,3.34615024548552));
#7005=CARTESIAN_POINT('Ctrl Pts',(-2.11507651911636,32.6218000776565,3.01218270613711));
#7006=CARTESIAN_POINT('Ctrl Pts',(-2.79836296968137,32.7468000776565,2.10293946007882));
#7007=CARTESIAN_POINT('Ctrl Pts',(-3.48164942024637,32.8718000776565,1.19369621402054));
#7008=CARTESIAN_POINT('Ctrl Pts',(-3.5,32.9968000776565,0.0564772772053689));
#7009=CARTESIAN_POINT('Ctrl Pts',(-3.51835057975363,33.1218000776565,-1.0807416596098));
#7010=CARTESIAN_POINT('Ctrl Pts',(-2.86475599094327,33.2468000776565,-2.01155730596849));
#7011=CARTESIAN_POINT('Ctrl Pts',(-2.2111614021329,33.3718000776565,-2.94237295232717));
#7012=CARTESIAN_POINT('Ctrl Pts',(-1.13527256282109,33.4968000776565,-3.31124536858055));
#7013=CARTESIAN_POINT('Ctrl Pts',(-0.0593837235092786,33.6218000776565,
-3.68011778483394));
#7014=CARTESIAN_POINT('Ctrl Pts',(1.02784639780354,33.7468000776565,-3.34615024548552));
#7015=CARTESIAN_POINT('Ctrl Pts',(2.11507651911636,33.8718000776565,-3.01218270613711));
#7016=CARTESIAN_POINT('Ctrl Pts',(2.79836296968137,33.9968000776565,-2.10293946007882));
#7017=CARTESIAN_POINT('Ctrl Pts',(3.48164942024637,34.1218000776565,-1.19369621402054));
#7018=CARTESIAN_POINT('Ctrl Pts',(3.5,34.2468000776565,-0.0564772772053694));
#7019=CARTESIAN_POINT('Ctrl Pts',(3.51835057975363,34.3718000776565,1.0807416596098));
#7020=CARTESIAN_POINT('Ctrl Pts',(2.86475599094327,34.4968000776565,2.01155730596849));
#7021=CARTESIAN_POINT('Ctrl Pts',(2.2111614021329,34.6218000776565,2.94237295232717));
#7022=CARTESIAN_POINT('Ctrl Pts',(1.13527256282109,34.7468000776565,3.31124536858055));
#7023=CARTESIAN_POINT('Ctrl Pts',(0.0593837235092791,34.8718000776565,3.68011778483394));
#7024=CARTESIAN_POINT('Ctrl Pts',(-1.02784639780354,34.9968000776565,3.34615024548552));
#7025=CARTESIAN_POINT('Ctrl Pts',(-2.11507651911636,35.1218000776565,3.01218270613711));
#7026=CARTESIAN_POINT('Ctrl Pts',(-2.79836296968137,35.2468000776565,2.10293946007882));
#7027=CARTESIAN_POINT('Ctrl Pts',(-3.48164942024637,35.3718000776565,1.19369621402054));
#7028=CARTESIAN_POINT('Ctrl Pts',(-3.5,35.4968000776565,0.0564772772053689));
#7029=CARTESIAN_POINT('Ctrl Pts',(-3.51835057975363,35.6218000776565,-1.0807416596098));
#7030=CARTESIAN_POINT('Ctrl Pts',(-2.86475599094327,35.7468000776565,-2.01155730596849));
#7031=CARTESIAN_POINT('Ctrl Pts',(-2.2111614021329,35.8718000776565,-2.94237295232717));
#7032=CARTESIAN_POINT('Ctrl Pts',(-1.13527256282109,35.9968000776565,-3.31124536858055));
#7033=CARTESIAN_POINT('Ctrl Pts',(-0.0593837235092786,36.1218000776565,
-3.68011778483394));
#7034=CARTESIAN_POINT('Ctrl Pts',(1.02784639780354,36.2468000776565,-3.34615024548552));
#7035=CARTESIAN_POINT('Ctrl Pts',(2.11507651911636,36.3718000776565,-3.01218270613711));
#7036=CARTESIAN_POINT('Ctrl Pts',(2.79836296968137,36.4968000776565,-2.10293946007882));
#7037=CARTESIAN_POINT('Ctrl Pts',(3.48164942024637,36.6218000776565,-1.19369621402054));
#7038=CARTESIAN_POINT('Ctrl Pts',(3.5,36.7468000776565,-0.0564772772053694));
#7039=CARTESIAN_POINT('Ctrl Pts',(3.51835057975363,36.8718000776565,1.0807416596098));
#7040=CARTESIAN_POINT('Ctrl Pts',(2.86475599094327,36.9968000776565,2.01155730596849));
#7041=CARTESIAN_POINT('Ctrl Pts',(2.2111614021329,37.1218000776565,2.94237295232717));
#7042=CARTESIAN_POINT('Ctrl Pts',(1.13527256282109,37.2468000776565,3.31124536858055));
#7043=CARTESIAN_POINT('Ctrl Pts',(0.0593837235092791,37.3718000776565,3.68011778483394));
#7044=CARTESIAN_POINT('Ctrl Pts',(-1.02784639780354,37.4968000776565,3.34615024548552));
#7045=CARTESIAN_POINT('Ctrl Pts',(-2.11507651911636,37.6218000776565,3.01218270613711));
#7046=CARTESIAN_POINT('Ctrl Pts',(-2.79836296968137,37.7468000776565,2.10293946007882));
#7047=CARTESIAN_POINT('Ctrl Pts',(-3.48164942024637,37.8718000776565,1.19369621402054));
#7048=CARTESIAN_POINT('Ctrl Pts',(-3.5,37.9968000776565,0.0564772772053689));
#7049=CARTESIAN_POINT('Ctrl Pts',(-3.51835057975363,38.1218000776565,-1.0807416596098));
#7050=CARTESIAN_POINT('Ctrl Pts',(-2.86475599094327,38.2468000776565,-2.01155730596849));
#7051=CARTESIAN_POINT('Ctrl Pts',(-2.2111614021329,38.3718000776565,-2.94237295232717));
#7052=CARTESIAN_POINT('Ctrl Pts',(-1.13527256282109,38.4968000776565,-3.31124536858055));
#7053=CARTESIAN_POINT('Ctrl Pts',(-0.0593837235092786,38.6218000776565,
-3.68011778483394));
#7054=CARTESIAN_POINT('Ctrl Pts',(1.02784639780354,38.7468000776565,-3.34615024548552));
#7055=CARTESIAN_POINT('Ctrl Pts',(2.11507651911636,38.8718000776565,-3.01218270613711));
#7056=CARTESIAN_POINT('Ctrl Pts',(2.79836296968137,38.9968000776565,-2.10293946007882));
#7057=CARTESIAN_POINT('Ctrl Pts',(3.48164942024637,39.1218000776565,-1.19369621402054));
#7058=CARTESIAN_POINT('Ctrl Pts',(3.5,39.2468000776565,-0.0564772772053694));
#7059=CARTESIAN_POINT('Ctrl Pts',(3.51835057975363,39.3718000776565,1.0807416596098));
#7060=CARTESIAN_POINT('Ctrl Pts',(2.86475599094327,39.4968000776565,2.01155730596849));
#7061=CARTESIAN_POINT('Ctrl Pts',(2.2111614021329,39.6218000776565,2.94237295232717));
#7062=CARTESIAN_POINT('Ctrl Pts',(1.13527256282109,39.7468000776565,3.31124536858055));
#7063=CARTESIAN_POINT('Ctrl Pts',(0.0593837235092791,39.8718000776565,3.68011778483394));
#7064=CARTESIAN_POINT('Ctrl Pts',(-1.02784639780354,39.9968000776565,3.34615024548552));
#7065=CARTESIAN_POINT('Ctrl Pts',(-2.11507651911636,40.1218000776565,3.01218270613711));
#7066=CARTESIAN_POINT('Ctrl Pts',(-2.79836296968137,40.2468000776565,2.10293946007882));
#7067=CARTESIAN_POINT('Ctrl Pts',(-3.48164942024637,40.3718000776565,1.19369621402054));
#7068=CARTESIAN_POINT('Ctrl Pts',(-3.5,40.4968000776565,0.0564772772053689));
#7069=CARTESIAN_POINT('Ctrl Pts',(-4.,15.,4.06619182768964E-14));
#7070=CARTESIAN_POINT('Ctrl Pts',(-4.,15.,-0.440632020643727));
#7071=CARTESIAN_POINT('Ctrl Pts',(-3.92185965933852,15.0000000000976,-0.877629741799447));
#7072=CARTESIAN_POINT('Ctrl Pts',(-3.62979221219699,15.0000000000976,-1.66011634884888));
#7073=CARTESIAN_POINT('Ctrl Pts',(-3.43268623534794,15.,-2.00518450039358));
#7074=CARTESIAN_POINT('Ctrl Pts',(-2.88759998961772,15.,-2.67411379288896));
#7075=CARTESIAN_POINT('Ctrl Pts',(-2.5779848430817,15.,-2.90941676657201));
#7076=CARTESIAN_POINT('Ctrl Pts',(-2.01365919589359,15.,-3.24428371091136));
#7077=CARTESIAN_POINT('Ctrl Pts',(-1.72921866213227,15.,-3.34220683205328));
#7078=CARTESIAN_POINT('Ctrl Pts',(-1.36507732602257,15.,-3.41070229712197));
#7079=CARTESIAN_POINT('Ctrl Pts',(-1.24715486254448,15.,-3.41477569775386));
#7080=CARTESIAN_POINT('Ctrl Pts',(-1.14129294530342,15.,-3.39661359285216));
#7081=CARTESIAN_POINT('Ctrl Pts',(-1.11145580616616,14.9999999999902,-3.38885059559076));
#7082=CARTESIAN_POINT('Ctrl Pts',(-1.08075410559423,14.9999999999902,-3.37025735211956));
#7083=CARTESIAN_POINT('Ctrl Pts',(-1.07322843619766,15.,-3.36443481553715));
#7084=CARTESIAN_POINT('Ctrl Pts',(-1.06203758490191,15.,-3.3514938315438));
#7085=CARTESIAN_POINT('Ctrl Pts',(-1.05807836132249,15.,-3.34489686808688));
#7086=CARTESIAN_POINT('Ctrl Pts',(-1.05560584366885,15.,-3.33749696414134));
#7087=CARTESIAN_POINT('Origin',(0.,15.,0.));
#7088=CARTESIAN_POINT('',(0.,0.,0.));
#7089=CARTESIAN_POINT('Origin',(-6.66666666666667,15.,20.5));
#7090=CARTESIAN_POINT('',(-6.66666666666667,10.,18.35));
#7091=CARTESIAN_POINT('Origin',(-6.66666666666667,10.,20.5));
#7092=CARTESIAN_POINT('',(-6.66666666666667,13.,18.35));
#7093=CARTESIAN_POINT('',(-6.66666666666667,15.,18.35));
#7094=CARTESIAN_POINT('Origin',(-6.66666666666667,13.,20.5));
#7095=CARTESIAN_POINT('Origin',(6.66666666666666,15.,20.5));
#7096=CARTESIAN_POINT('',(6.66666666666666,10.,18.35));
#7097=CARTESIAN_POINT('Origin',(6.66666666666666,10.,20.5));
#7098=CARTESIAN_POINT('',(6.66666666666666,13.,18.35));
#7099=CARTESIAN_POINT('',(6.66666666666666,15.,18.35));
#7100=CARTESIAN_POINT('Origin',(6.66666666666666,13.,20.5));
#7101=CARTESIAN_POINT('Origin',(6.66666666666666,15.,-20.5));
#7102=CARTESIAN_POINT('',(6.66666666666666,10.,-22.65));
#7103=CARTESIAN_POINT('Origin',(6.66666666666666,10.,-20.5));
#7104=CARTESIAN_POINT('',(6.66666666666666,13.,-22.65));
#7105=CARTESIAN_POINT('',(6.66666666666666,15.,-22.65));
#7106=CARTESIAN_POINT('Origin',(6.66666666666666,13.,-20.5));
#7107=CARTESIAN_POINT('Origin',(-6.66666666666667,15.,-20.5));
#7108=CARTESIAN_POINT('',(-6.66666666666667,10.,-22.65));
#7109=CARTESIAN_POINT('Origin',(-6.66666666666667,10.,-20.5));
#7110=CARTESIAN_POINT('',(-6.66666666666667,13.,-22.65));
#7111=CARTESIAN_POINT('',(-6.66666666666667,15.,-22.65));
#7112=CARTESIAN_POINT('Origin',(-6.66666666666667,13.,-20.5));
#7113=CARTESIAN_POINT('Origin',(8.67361737988404E-15,13.,3.46944695195361E-15));
#7114=CARTESIAN_POINT('',(7.81636462048089E-15,13.,7.));
#7115=CARTESIAN_POINT('Origin',(8.67361737988404E-15,13.,3.46944695195361E-15));
#7116=CARTESIAN_POINT('',(7.81636462048089E-15,10.,7.));
#7117=CARTESIAN_POINT('',(7.81636462048089E-15,13.,7.));
#7118=CARTESIAN_POINT('Origin',(8.67361737988404E-15,10.,3.46944695195361E-15));
#7119=CARTESIAN_POINT('Origin',(0.,10.,0.));
#7120=CARTESIAN_POINT('',(15.,10.,25.));
#7121=CARTESIAN_POINT('',(15.,10.,-25.));
#7122=CARTESIAN_POINT('',(15.,10.,25.));
#7123=CARTESIAN_POINT('',(-15.,10.,25.));
#7124=CARTESIAN_POINT('',(-15.,10.,25.));
#7125=CARTESIAN_POINT('',(-15.,10.,-25.));
#7126=CARTESIAN_POINT('',(-15.,10.,25.));
#7127=CARTESIAN_POINT('',(-15.,10.,-25.));
#7128=CARTESIAN_POINT('Origin',(0.,13.,0.));
#7129=CARTESIAN_POINT('',(15.,13.,25.));
#7130=CARTESIAN_POINT('',(15.,13.,-25.));
#7131=CARTESIAN_POINT('',(15.,13.,25.));
#7132=CARTESIAN_POINT('',(-15.,13.,-25.));
#7133=CARTESIAN_POINT('',(-15.,13.,-25.));
#7134=CARTESIAN_POINT('',(-15.,13.,25.));
#7135=CARTESIAN_POINT('',(-15.,13.,25.));
#7136=CARTESIAN_POINT('',(-15.,13.,25.));
#7137=CARTESIAN_POINT('Origin',(15.,13.,25.));
#7138=CARTESIAN_POINT('',(15.,13.,-25.));
#7139=CARTESIAN_POINT('',(15.,13.,25.));
#7140=CARTESIAN_POINT('Origin',(-15.,13.,-25.));
#7141=CARTESIAN_POINT('',(-15.,13.,-25.));
#7142=CARTESIAN_POINT('Origin',(-15.,13.,25.));
#7143=CARTESIAN_POINT('',(-15.,13.,25.));
#7144=CARTESIAN_POINT('Origin',(-15.,13.,25.));
#7145=CARTESIAN_POINT('',(0.,0.,0.));
#7146=CARTESIAN_POINT('Origin',(0.,43.,0.));
#7147=CARTESIAN_POINT('',(-7.96020419445779E-16,43.,6.5));
#7148=CARTESIAN_POINT('Origin',(0.,43.,0.));
#7149=CARTESIAN_POINT('',(-7.96020419445779E-16,13.,6.5));
#7150=CARTESIAN_POINT('',(-7.96020419445779E-16,43.,6.5));
#7151=CARTESIAN_POINT('Origin',(0.,13.,0.));
#7152=CARTESIAN_POINT('Origin',(-9.18485099360515E-16,43.,-2.5));
#7153=CARTESIAN_POINT('',(8.,46.,-2.5));
#7154=CARTESIAN_POINT('',(-8.,46.,-2.5));
#7155=CARTESIAN_POINT('Origin',(-9.18485099360515E-16,46.,-2.5));
#7156=CARTESIAN_POINT('',(8.,13.,-2.5));
#7157=CARTESIAN_POINT('',(8.,43.,-2.5));
#7158=CARTESIAN_POINT('',(-8.,13.,-2.5));
#7159=CARTESIAN_POINT('Origin',(-9.18485099360515E-16,13.,-2.5));
#7160=CARTESIAN_POINT('',(-8.,43.,-2.5));
#7161=CARTESIAN_POINT('Origin',(0.,13.,2.5));
#7162=CARTESIAN_POINT('',(-8.,13.,2.5));
#7163=CARTESIAN_POINT('',(8.,13.,2.5));
#7164=CARTESIAN_POINT('Origin',(0.,13.,2.5));
#7165=CARTESIAN_POINT('',(-8.,13.,2.5));
#7166=CARTESIAN_POINT('',(8.,13.,2.5));
#7167=CARTESIAN_POINT('Origin',(0.,43.,2.5));
#7168=CARTESIAN_POINT('',(8.,46.,2.5));
#7169=CARTESIAN_POINT('',(8.,43.,2.5));
#7170=CARTESIAN_POINT('',(-8.,46.,2.5));
#7171=CARTESIAN_POINT('Origin',(0.,46.,2.5));
#7172=CARTESIAN_POINT('',(-8.,43.,2.5));
#7173=CARTESIAN_POINT('Origin',(8.,43.,2.5));
#7174=CARTESIAN_POINT('',(8.,46.,2.5));
#7175=CARTESIAN_POINT('Origin',(-8.,43.,2.5));
#7176=CARTESIAN_POINT('',(-8.,46.,2.5));
#7177=CARTESIAN_POINT('Origin',(0.,43.,2.5));
#7178=CARTESIAN_POINT('Origin',(0.,46.,2.5));
#7179=CARTESIAN_POINT('',(0.,0.,0.));
#7180=CARTESIAN_POINT('Origin',(0.,43.,2.5));
#7181=CARTESIAN_POINT('',(-8.,43.,2.5));
#7182=CARTESIAN_POINT('Origin',(-9.,43.,2.5));
#7183=CARTESIAN_POINT('',(8.00000000000001,43.,2.5));
#7184=CARTESIAN_POINT('Origin',(0.,43.,2.5));
#7185=CARTESIAN_POINT('Origin',(9.00000000000001,43.,2.5));
#7186=CARTESIAN_POINT('Origin',(-1.73472347597681E-15,43.,-2.5));
#7187=CARTESIAN_POINT('',(8.,43.,-2.5));
#7188=CARTESIAN_POINT('Origin',(9.,43.,-2.5));
#7189=CARTESIAN_POINT('',(-8.,43.,-2.5));
#7190=CARTESIAN_POINT('Origin',(-1.73472347597681E-15,43.,-2.5));
#7191=CARTESIAN_POINT('Origin',(-9.,43.,-2.5));
#7192=CARTESIAN_POINT('Origin',(-9.,43.,2.5));
#7193=CARTESIAN_POINT('',(-8.,43.,2.5));
#7194=CARTESIAN_POINT('Origin',(9.,43.,-2.5));
#7195=CARTESIAN_POINT('',(8.,43.,-2.5));
#7196=CARTESIAN_POINT('Origin',(0.,40.8,2.5));
#7197=CARTESIAN_POINT('',(-8.,40.8,2.5));
#7198=CARTESIAN_POINT('Origin',(-9.,40.8,2.5));
#7199=CARTESIAN_POINT('',(8.00000000000001,40.8,2.5));
#7200=CARTESIAN_POINT('Origin',(0.,40.8,2.5));
#7201=CARTESIAN_POINT('Origin',(9.00000000000001,40.8,2.5));
#7202=CARTESIAN_POINT('Origin',(-1.73472347597681E-15,40.8,-2.5));
#7203=CARTESIAN_POINT('',(8.,40.8,-2.5));
#7204=CARTESIAN_POINT('Origin',(9.,40.8,-2.5));
#7205=CARTESIAN_POINT('',(-8.,40.8,-2.5));
#7206=CARTESIAN_POINT('Origin',(-1.73472347597681E-15,40.8,-2.5));
#7207=CARTESIAN_POINT('Origin',(-9.,40.8,-2.5));
#7208=CARTESIAN_POINT('Origin',(-9.,40.8,2.5));
#7209=CARTESIAN_POINT('',(-8.,40.8,2.5));
#7210=CARTESIAN_POINT('Origin',(9.,40.8,-2.5));
#7211=CARTESIAN_POINT('',(8.,40.8,-2.5));
#7212=CARTESIAN_POINT('Origin',(0.,38.6,2.5));
#7213=CARTESIAN_POINT('',(-8.,38.6,2.5));
#7214=CARTESIAN_POINT('Origin',(-9.,38.6,2.5));
#7215=CARTESIAN_POINT('',(8.00000000000001,38.6,2.5));
#7216=CARTESIAN_POINT('Origin',(0.,38.6,2.5));
#7217=CARTESIAN_POINT('Origin',(9.00000000000001,38.6,2.5));
#7218=CARTESIAN_POINT('Origin',(-1.73472347597681E-15,38.6,-2.5));
#7219=CARTESIAN_POINT('',(8.,38.6,-2.5));
#7220=CARTESIAN_POINT('Origin',(9.,38.6,-2.5));
#7221=CARTESIAN_POINT('',(-8.,38.6,-2.5));
#7222=CARTESIAN_POINT('Origin',(-1.73472347597681E-15,38.6,-2.5));
#7223=CARTESIAN_POINT('Origin',(-9.,38.6,-2.5));
#7224=CARTESIAN_POINT('Origin',(-9.,38.6,2.5));
#7225=CARTESIAN_POINT('',(-8.,38.6,2.5));
#7226=CARTESIAN_POINT('Origin',(9.,38.6,-2.5));
#7227=CARTESIAN_POINT('',(8.,38.6,-2.5));
#7228=CARTESIAN_POINT('Origin',(0.,36.4,2.5));
#7229=CARTESIAN_POINT('',(-8.,36.4,2.5));
#7230=CARTESIAN_POINT('Origin',(-9.,36.4,2.5));
#7231=CARTESIAN_POINT('',(8.00000000000001,36.4,2.5));
#7232=CARTESIAN_POINT('Origin',(0.,36.4,2.5));
#7233=CARTESIAN_POINT('Origin',(9.00000000000001,36.4,2.5));
#7234=CARTESIAN_POINT('Origin',(-1.73472347597681E-15,36.4,-2.5));
#7235=CARTESIAN_POINT('',(8.,36.4,-2.5));
#7236=CARTESIAN_POINT('Origin',(9.,36.4,-2.5));
#7237=CARTESIAN_POINT('',(-8.,36.4,-2.5));
#7238=CARTESIAN_POINT('Origin',(-1.73472347597681E-15,36.4,-2.5));
#7239=CARTESIAN_POINT('Origin',(-9.,36.4,-2.5));
#7240=CARTESIAN_POINT('Origin',(-9.,36.4,2.5));
#7241=CARTESIAN_POINT('',(-8.,36.4,2.5));
#7242=CARTESIAN_POINT('Origin',(9.,36.4,-2.5));
#7243=CARTESIAN_POINT('',(8.,36.4,-2.5));
#7244=CARTESIAN_POINT('Origin',(0.,34.2,2.5));
#7245=CARTESIAN_POINT('',(-8.,34.2,2.5));
#7246=CARTESIAN_POINT('Origin',(-9.,34.2,2.5));
#7247=CARTESIAN_POINT('',(8.00000000000001,34.2,2.5));
#7248=CARTESIAN_POINT('Origin',(0.,34.2,2.5));
#7249=CARTESIAN_POINT('Origin',(9.00000000000001,34.2,2.5));
#7250=CARTESIAN_POINT('Origin',(-1.73472347597681E-15,34.2,-2.5));
#7251=CARTESIAN_POINT('',(8.,34.2,-2.5));
#7252=CARTESIAN_POINT('Origin',(9.,34.2,-2.5));
#7253=CARTESIAN_POINT('',(-8.,34.2,-2.5));
#7254=CARTESIAN_POINT('Origin',(-1.73472347597681E-15,34.2,-2.5));
#7255=CARTESIAN_POINT('Origin',(-9.,34.2,-2.5));
#7256=CARTESIAN_POINT('Origin',(-9.,34.2,2.5));
#7257=CARTESIAN_POINT('',(-8.,34.2,2.5));
#7258=CARTESIAN_POINT('Origin',(9.,34.2,-2.5));
#7259=CARTESIAN_POINT('',(8.,34.2,-2.5));
#7260=CARTESIAN_POINT('Origin',(0.,32.,2.5));
#7261=CARTESIAN_POINT('',(-8.,32.,2.5));
#7262=CARTESIAN_POINT('Origin',(-9.,32.,2.5));
#7263=CARTESIAN_POINT('',(8.00000000000001,32.,2.5));
#7264=CARTESIAN_POINT('Origin',(0.,32.,2.5));
#7265=CARTESIAN_POINT('Origin',(9.00000000000001,32.,2.5));
#7266=CARTESIAN_POINT('Origin',(-1.73472347597681E-15,32.,-2.5));
#7267=CARTESIAN_POINT('',(8.,32.,-2.5));
#7268=CARTESIAN_POINT('Origin',(9.,32.,-2.5));
#7269=CARTESIAN_POINT('',(-8.,32.,-2.5));
#7270=CARTESIAN_POINT('Origin',(-1.73472347597681E-15,32.,-2.5));
#7271=CARTESIAN_POINT('Origin',(-9.,32.,-2.5));
#7272=CARTESIAN_POINT('Origin',(-9.,32.,2.5));
#7273=CARTESIAN_POINT('',(-8.,32.,2.5));
#7274=CARTESIAN_POINT('Origin',(9.,32.,-2.5));
#7275=CARTESIAN_POINT('',(8.,32.,-2.5));
#7276=CARTESIAN_POINT('Origin',(0.,29.8,2.5));
#7277=CARTESIAN_POINT('',(-8.,29.8,2.5));
#7278=CARTESIAN_POINT('Origin',(-9.,29.8,2.5));
#7279=CARTESIAN_POINT('',(8.00000000000001,29.8,2.5));
#7280=CARTESIAN_POINT('Origin',(0.,29.8,2.5));
#7281=CARTESIAN_POINT('Origin',(9.00000000000001,29.8,2.5));
#7282=CARTESIAN_POINT('Origin',(-1.73472347597681E-15,29.8,-2.5));
#7283=CARTESIAN_POINT('',(8.,29.8,-2.5));
#7284=CARTESIAN_POINT('Origin',(9.,29.8,-2.5));
#7285=CARTESIAN_POINT('',(-8.,29.8,-2.5));
#7286=CARTESIAN_POINT('Origin',(-1.73472347597681E-15,29.8,-2.5));
#7287=CARTESIAN_POINT('Origin',(-9.,29.8,-2.5));
#7288=CARTESIAN_POINT('Origin',(-9.,29.8,2.5));
#7289=CARTESIAN_POINT('',(-8.,29.8,2.5));
#7290=CARTESIAN_POINT('Origin',(9.,29.8,-2.5));
#7291=CARTESIAN_POINT('',(8.,29.8,-2.5));
#7292=CARTESIAN_POINT('Origin',(0.,27.6,2.5));
#7293=CARTESIAN_POINT('',(-8.,27.6,2.5));
#7294=CARTESIAN_POINT('Origin',(-9.,27.6,2.5));
#7295=CARTESIAN_POINT('',(8.00000000000001,27.6,2.5));
#7296=CARTESIAN_POINT('Origin',(0.,27.6,2.5));
#7297=CARTESIAN_POINT('Origin',(9.00000000000001,27.6,2.5));
#7298=CARTESIAN_POINT('Origin',(-1.73472347597681E-15,27.6,-2.5));
#7299=CARTESIAN_POINT('',(8.,27.6,-2.5));
#7300=CARTESIAN_POINT('Origin',(9.,27.6,-2.5));
#7301=CARTESIAN_POINT('',(-8.,27.6,-2.5));
#7302=CARTESIAN_POINT('Origin',(-1.73472347597681E-15,27.6,-2.5));
#7303=CARTESIAN_POINT('Origin',(-9.,27.6,-2.5));
#7304=CARTESIAN_POINT('Origin',(-9.,27.6,2.5));
#7305=CARTESIAN_POINT('',(-8.,27.6,2.5));
#7306=CARTESIAN_POINT('Origin',(9.,27.6,-2.5));
#7307=CARTESIAN_POINT('',(8.,27.6,-2.5));
#7308=CARTESIAN_POINT('Origin',(0.,25.4,2.5));
#7309=CARTESIAN_POINT('',(-8.,25.4,2.5));
#7310=CARTESIAN_POINT('Origin',(-9.,25.4,2.5));
#7311=CARTESIAN_POINT('',(8.00000000000001,25.4,2.5));
#7312=CARTESIAN_POINT('Origin',(0.,25.4,2.5));
#7313=CARTESIAN_POINT('Origin',(9.00000000000001,25.4,2.5));
#7314=CARTESIAN_POINT('Origin',(-1.73472347597681E-15,25.4,-2.5));
#7315=CARTESIAN_POINT('',(8.,25.4,-2.5));
#7316=CARTESIAN_POINT('Origin',(9.,25.4,-2.5));
#7317=CARTESIAN_POINT('',(-8.,25.4,-2.5));
#7318=CARTESIAN_POINT('Origin',(-1.73472347597681E-15,25.4,-2.5));
#7319=CARTESIAN_POINT('Origin',(-9.,25.4,-2.5));
#7320=CARTESIAN_POINT('Origin',(-9.,25.4,2.5));
#7321=CARTESIAN_POINT('',(-8.,25.4,2.5));
#7322=CARTESIAN_POINT('Origin',(9.,25.4,-2.5));
#7323=CARTESIAN_POINT('',(8.,25.4,-2.5));
#7324=CARTESIAN_POINT('Origin',(0.,23.2,2.5));
#7325=CARTESIAN_POINT('',(-8.,23.2,2.5));
#7326=CARTESIAN_POINT('Origin',(-9.,23.2,2.5));
#7327=CARTESIAN_POINT('',(8.00000000000001,23.2,2.5));
#7328=CARTESIAN_POINT('Origin',(0.,23.2,2.5));
#7329=CARTESIAN_POINT('Origin',(9.00000000000001,23.2,2.5));
#7330=CARTESIAN_POINT('Origin',(-1.73472347597681E-15,23.2,-2.5));
#7331=CARTESIAN_POINT('',(8.,23.2,-2.5));
#7332=CARTESIAN_POINT('Origin',(9.,23.2,-2.5));
#7333=CARTESIAN_POINT('',(-8.,23.2,-2.5));
#7334=CARTESIAN_POINT('Origin',(-1.73472347597681E-15,23.2,-2.5));
#7335=CARTESIAN_POINT('Origin',(-9.,23.2,-2.5));
#7336=CARTESIAN_POINT('Origin',(-9.,23.2,2.5));
#7337=CARTESIAN_POINT('',(-8.,23.2,2.5));
#7338=CARTESIAN_POINT('Origin',(9.,23.2,-2.5));
#7339=CARTESIAN_POINT('',(8.,23.2,-2.5));
#7340=CARTESIAN_POINT('Origin',(0.,21.,2.5));
#7341=CARTESIAN_POINT('',(-8.,21.,2.5));
#7342=CARTESIAN_POINT('Origin',(-9.,21.,2.5));
#7343=CARTESIAN_POINT('',(8.00000000000001,21.,2.5));
#7344=CARTESIAN_POINT('Origin',(0.,21.,2.5));
#7345=CARTESIAN_POINT('Origin',(9.00000000000001,21.,2.5));
#7346=CARTESIAN_POINT('Origin',(-1.73472347597681E-15,21.,-2.5));
#7347=CARTESIAN_POINT('',(8.,21.,-2.5));
#7348=CARTESIAN_POINT('Origin',(9.,21.,-2.5));
#7349=CARTESIAN_POINT('',(-8.,21.,-2.5));
#7350=CARTESIAN_POINT('Origin',(-1.73472347597681E-15,21.,-2.5));
#7351=CARTESIAN_POINT('Origin',(-9.,21.,-2.5));
#7352=CARTESIAN_POINT('Origin',(-9.,21.,2.5));
#7353=CARTESIAN_POINT('',(-8.,21.,2.5));
#7354=CARTESIAN_POINT('Origin',(9.,21.,-2.5));
#7355=CARTESIAN_POINT('',(8.,21.,-2.5));
#7356=CARTESIAN_POINT('Origin',(0.,18.8,2.5));
#7357=CARTESIAN_POINT('',(-8.,18.8,2.5));
#7358=CARTESIAN_POINT('Origin',(-9.,18.8,2.5));
#7359=CARTESIAN_POINT('',(8.00000000000001,18.8,2.5));
#7360=CARTESIAN_POINT('Origin',(0.,18.8,2.5));
#7361=CARTESIAN_POINT('Origin',(9.00000000000001,18.8,2.5));
#7362=CARTESIAN_POINT('Origin',(-1.73472347597681E-15,18.8,-2.5));
#7363=CARTESIAN_POINT('',(8.,18.8,-2.5));
#7364=CARTESIAN_POINT('Origin',(9.,18.8,-2.5));
#7365=CARTESIAN_POINT('',(-8.,18.8,-2.5));
#7366=CARTESIAN_POINT('Origin',(-1.73472347597681E-15,18.8,-2.5));
#7367=CARTESIAN_POINT('Origin',(-9.,18.8,-2.5));
#7368=CARTESIAN_POINT('Origin',(-9.,18.8,2.5));
#7369=CARTESIAN_POINT('',(-8.,18.8,2.5));
#7370=CARTESIAN_POINT('Origin',(9.,18.8,-2.5));
#7371=CARTESIAN_POINT('',(8.,18.8,-2.5));
#7372=CARTESIAN_POINT('Origin',(0.,16.6,2.5));
#7373=CARTESIAN_POINT('',(-8.,16.6,2.5));
#7374=CARTESIAN_POINT('Origin',(-9.,16.6,2.5));
#7375=CARTESIAN_POINT('',(8.00000000000001,16.6,2.5));
#7376=CARTESIAN_POINT('Origin',(0.,16.6,2.5));
#7377=CARTESIAN_POINT('Origin',(9.00000000000001,16.6,2.5));
#7378=CARTESIAN_POINT('Origin',(-1.73472347597681E-15,16.6,-2.5));
#7379=CARTESIAN_POINT('',(8.,16.6,-2.5));
#7380=CARTESIAN_POINT('Origin',(9.,16.6,-2.5));
#7381=CARTESIAN_POINT('',(-8.,16.6,-2.5));
#7382=CARTESIAN_POINT('Origin',(-1.73472347597681E-15,16.6,-2.5));
#7383=CARTESIAN_POINT('Origin',(-9.,16.6,-2.5));
#7384=CARTESIAN_POINT('Origin',(-9.,16.6,2.5));
#7385=CARTESIAN_POINT('',(-8.,16.6,2.5));
#7386=CARTESIAN_POINT('Origin',(9.,16.6,-2.5));
#7387=CARTESIAN_POINT('',(8.,16.6,-2.5));
#7388=CARTESIAN_POINT('',(0.,0.,0.));
#7389=CARTESIAN_POINT('Origin',(-6.66666666666667,14.8,-20.5));
#7390=CARTESIAN_POINT('',(-6.66666666666667,14.9936491673104,-22.65));
#7391=CARTESIAN_POINT('Origin',(-6.66666666666667,14.9936491673104,-20.5));
#7392=CARTESIAN_POINT('',(-6.66666666666667,15.,-22.7));
#7393=CARTESIAN_POINT('Origin',(-6.66666666666667,14.8,-22.7));
#7394=CARTESIAN_POINT('Origin',(-6.66666666666667,15.,-20.5));
#7395=CARTESIAN_POINT('Origin',(6.66666666666666,14.8,-20.5));
#7396=CARTESIAN_POINT('',(6.66666666666666,14.9936491673104,-22.65));
#7397=CARTESIAN_POINT('Origin',(6.66666666666666,14.9936491673104,-20.5));
#7398=CARTESIAN_POINT('',(6.66666666666666,15.,-22.7));
#7399=CARTESIAN_POINT('Origin',(6.66666666666666,14.8,-22.7));
#7400=CARTESIAN_POINT('Origin',(6.66666666666666,15.,-20.5));
#7401=CARTESIAN_POINT('Origin',(6.66666666666666,14.8,20.5));
#7402=CARTESIAN_POINT('',(6.66666666666666,14.9936491673104,18.35));
#7403=CARTESIAN_POINT('Origin',(6.66666666666666,14.9936491673104,20.5));
#7404=CARTESIAN_POINT('',(6.66666666666666,15.,18.3));
#7405=CARTESIAN_POINT('Origin',(6.66666666666666,14.8,18.3));
#7406=CARTESIAN_POINT('Origin',(6.66666666666666,15.,20.5));
#7407=CARTESIAN_POINT('Origin',(-6.66666666666667,14.8,20.5));
#7408=CARTESIAN_POINT('',(-6.66666666666667,14.9936491673104,18.35));
#7409=CARTESIAN_POINT('Origin',(-6.66666666666667,14.9936491673104,20.5));
#7410=CARTESIAN_POINT('',(-6.66666666666667,15.,18.3));
#7411=CARTESIAN_POINT('Origin',(-6.66666666666667,14.8,18.3));
#7412=CARTESIAN_POINT('Origin',(-6.66666666666667,15.,20.5));
#7413=CARTESIAN_POINT('Origin',(-6.66666666666667,15.,20.5));
#7414=CARTESIAN_POINT('',(-6.66666666666667,13.,18.35));
#7415=CARTESIAN_POINT('Origin',(-6.66666666666667,13.,20.5));
#7416=CARTESIAN_POINT('',(-6.66666666666667,15.,18.35));
#7417=CARTESIAN_POINT('Origin',(6.66666666666666,15.,20.5));
#7418=CARTESIAN_POINT('',(6.66666666666666,13.,18.35));
#7419=CARTESIAN_POINT('Origin',(6.66666666666666,13.,20.5));
#7420=CARTESIAN_POINT('',(6.66666666666666,15.,18.35));
#7421=CARTESIAN_POINT('Origin',(6.66666666666666,15.,-20.5));
#7422=CARTESIAN_POINT('',(6.66666666666666,13.,-22.65));
#7423=CARTESIAN_POINT('Origin',(6.66666666666666,13.,-20.5));
#7424=CARTESIAN_POINT('',(6.66666666666666,15.,-22.65));
#7425=CARTESIAN_POINT('Origin',(-6.66666666666667,15.,-20.5));
#7426=CARTESIAN_POINT('',(-6.66666666666667,13.,-22.65));
#7427=CARTESIAN_POINT('Origin',(-6.66666666666667,13.,-20.5));
#7428=CARTESIAN_POINT('',(-6.66666666666667,15.,-22.65));
#7429=CARTESIAN_POINT('Origin',(0.,48.,-16.));
#7430=CARTESIAN_POINT('',(-13.,15.,-16.));
#7431=CARTESIAN_POINT('',(13.,15.,-16.));
#7432=CARTESIAN_POINT('',(-13.,15.,-16.));
#7433=CARTESIAN_POINT('',(-13.,49.,-16.));
#7434=CARTESIAN_POINT('',(-13.,48.,-16.));
#7435=CARTESIAN_POINT('',(13.,49.,-16.));
#7436=CARTESIAN_POINT('',(-13.,49.,-16.));
#7437=CARTESIAN_POINT('',(13.,48.,-16.));
#7438=CARTESIAN_POINT('Origin',(0.,48.,16.));
#7439=CARTESIAN_POINT('',(13.,15.,16.));
#7440=CARTESIAN_POINT('',(-13.,15.,16.));
#7441=CARTESIAN_POINT('',(-13.,15.,16.));
#7442=CARTESIAN_POINT('',(13.,49.,16.));
#7443=CARTESIAN_POINT('',(13.,48.,16.));
#7444=CARTESIAN_POINT('',(-13.,49.,16.));
#7445=CARTESIAN_POINT('',(-13.,49.,16.));
#7446=CARTESIAN_POINT('',(-13.,48.,16.));
#7447=CARTESIAN_POINT('Origin',(0.,13.,0.));
#7448=CARTESIAN_POINT('',(13.,13.,25.));
#7449=CARTESIAN_POINT('',(13.,13.,-25.));
#7450=CARTESIAN_POINT('',(13.,13.,0.));
#7451=CARTESIAN_POINT('',(-13.,13.,25.));
#7452=CARTESIAN_POINT('',(-13.,13.,25.));
#7453=CARTESIAN_POINT('',(-13.,13.,-25.));
#7454=CARTESIAN_POINT('',(-13.,13.,0.));
#7455=CARTESIAN_POINT('',(-13.,13.,-25.));
#7456=CARTESIAN_POINT('',(12.,13.,15.));
#7457=CARTESIAN_POINT('',(12.,13.,-15.));
#7458=CARTESIAN_POINT('',(12.,13.,15.));
#7459=CARTESIAN_POINT('',(-12.,13.,-15.));
#7460=CARTESIAN_POINT('',(-12.,13.,-15.));
#7461=CARTESIAN_POINT('',(-12.,13.,15.));
#7462=CARTESIAN_POINT('',(-12.,13.,15.));
#7463=CARTESIAN_POINT('',(-12.,13.,15.));
#7464=CARTESIAN_POINT('Origin',(13.,48.,0.));
#7465=CARTESIAN_POINT('',(13.,15.,-25.));
#7466=CARTESIAN_POINT('',(13.,15.,-25.));
#7467=CARTESIAN_POINT('',(13.,15.,-16.));
#7468=CARTESIAN_POINT('',(13.,49.,16.));
#7469=CARTESIAN_POINT('',(13.,15.,25.));
#7470=CARTESIAN_POINT('',(13.,15.,16.));
#7471=CARTESIAN_POINT('',(13.,15.,25.));
#7472=CARTESIAN_POINT('Origin',(-13.,48.,0.));
#7473=CARTESIAN_POINT('',(-13.,15.,25.));
#7474=CARTESIAN_POINT('',(-13.,15.,25.));
#7475=CARTESIAN_POINT('',(-13.,15.,16.));
#7476=CARTESIAN_POINT('',(-13.,49.,16.));
#7477=CARTESIAN_POINT('',(-13.,15.,-25.));
#7478=CARTESIAN_POINT('',(-13.,15.,-16.));
#7479=CARTESIAN_POINT('',(-13.,15.,-25.));
#7480=CARTESIAN_POINT('Origin',(12.,48.,15.));
#7481=CARTESIAN_POINT('',(12.,48.,15.));
#7482=CARTESIAN_POINT('',(12.,48.,15.));
#7483=CARTESIAN_POINT('',(12.,48.,-15.));
#7484=CARTESIAN_POINT('',(12.,48.,15.));
#7485=CARTESIAN_POINT('',(12.,48.,-15.));
#7486=CARTESIAN_POINT('Origin',(-12.,48.,-15.));
#7487=CARTESIAN_POINT('',(-12.,48.,-15.));
#7488=CARTESIAN_POINT('',(-12.,48.,-15.));
#7489=CARTESIAN_POINT('',(-12.,48.,-15.));
#7490=CARTESIAN_POINT('Origin',(-12.,48.,15.));
#7491=CARTESIAN_POINT('',(-12.,48.,15.));
#7492=CARTESIAN_POINT('',(-12.,48.,15.));
#7493=CARTESIAN_POINT('',(-12.,48.,15.));
#7494=CARTESIAN_POINT('Origin',(-12.,48.,15.));
#7495=CARTESIAN_POINT('',(-12.,48.,15.));
#7496=CARTESIAN_POINT('Origin',(0.,48.,0.));
#7497=CARTESIAN_POINT('Origin',(0.,49.,0.));
#7498=CARTESIAN_POINT('Origin',(-13.,15.,25.));
#7499=CARTESIAN_POINT('',(-13.,15.,25.));
#7500=CARTESIAN_POINT('Origin',(0.,15.,0.));
#7501=CARTESIAN_POINT('Origin',(-13.,15.,-25.));
#7502=CARTESIAN_POINT('',(-13.,15.,-25.));
#7503=CARTESIAN_POINT('Origin',(0.,15.,0.));
#7504=CARTESIAN_POINT('',(0.,0.,0.));
#7505=CARTESIAN_POINT('Origin',(-997.978312163513,0.,0.));
#7506=CARTESIAN_POINT('',(2.02168783648704,2.16840434497101E-16,0.));
#7507=CARTESIAN_POINT('',(1.3,0.,-1.25));
#7508=CARTESIAN_POINT('',(-997.978312163513,-2.12115047744979E-13,-1732.05080756886));
#7509=CARTESIAN_POINT('',(1.3,-1.08253175473055,-0.625));
#7510=CARTESIAN_POINT('Origin',(1.3,0.,0.));
#7511=CARTESIAN_POINT('',(1.3,-1.08253175473055,0.625));
#7512=CARTESIAN_POINT('Origin',(1.3,0.,0.));
#7513=CARTESIAN_POINT('',(1.3,1.87789324842145E-16,1.25));
#7514=CARTESIAN_POINT('Origin',(1.3,0.,0.));
#7515=CARTESIAN_POINT('',(1.3,1.08253175473055,0.625000000000001));
#7516=CARTESIAN_POINT('Origin',(1.3,0.,0.));
#7517=CARTESIAN_POINT('',(1.3,1.08253175473055,-0.625));
#7518=CARTESIAN_POINT('Origin',(1.3,0.,0.));
#7519=CARTESIAN_POINT('Origin',(1.3,0.,0.));
#7520=CARTESIAN_POINT('Origin',(2.4,0.,0.));
#7521=CARTESIAN_POINT('',(2.2,-2.69422295812418E-16,-2.2));
#7522=CARTESIAN_POINT('Origin',(2.2,0.,0.));
#7523=CARTESIAN_POINT('',(2.4,-2.44929359829471E-16,-2.));
#7524=CARTESIAN_POINT('Origin',(2.4,-2.69422295812418E-16,-2.2));
#7525=CARTESIAN_POINT('Origin',(2.4,0.,0.));
#7526=CARTESIAN_POINT('Origin',(14.2,0.,0.));
#7527=CARTESIAN_POINT('',(13.81,-2.44929359829471E-16,-2.));
#7528=CARTESIAN_POINT('Origin',(13.81,0.,0.));
#7529=CARTESIAN_POINT('',(14.2,-1.97168134662724E-16,-1.61));
#7530=CARTESIAN_POINT('',(14.2,-1.97168134662724E-16,-1.61));
#7531=CARTESIAN_POINT('Origin',(14.2,0.,0.));
#7532=CARTESIAN_POINT('Origin',(0.,0.,0.));
#7533=CARTESIAN_POINT('',(0.,-2.44929359829471E-16,-2.));
#7534=CARTESIAN_POINT('Origin',(0.,0.,0.));
#7535=CARTESIAN_POINT('',(1.82,-4.65365783675994E-16,-3.8));
#7536=CARTESIAN_POINT('Origin',(1.82,0.,0.));
#7537=CARTESIAN_POINT('',(2.2,-4.65365783675994E-16,-3.8));
#7538=CARTESIAN_POINT('',(0.,-4.65365783675994E-16,-3.8));
#7539=CARTESIAN_POINT('Origin',(2.2,0.,0.));
#7540=CARTESIAN_POINT('Origin',(3.88527472527473,-4.33680868994202E-16,
0.));
#7541=CARTESIAN_POINT('',(8.67361737988404E-16,1.9,0.));
#7542=CARTESIAN_POINT('Origin',(8.67361737988404E-16,0.,0.));
#7543=CARTESIAN_POINT('Origin',(4.33680868994202E-16,0.,0.));
#7544=CARTESIAN_POINT('',(0.,0.721687836487033,1.25));
#7545=CARTESIAN_POINT('',(4.33680868994202E-16,-0.721687836487032,1.25));
#7546=CARTESIAN_POINT('',(0.,-0.721687836487032,1.25));
#7547=CARTESIAN_POINT('',(0.,-1.44337567297406,1.27850268845987E-18));
#7548=CARTESIAN_POINT('',(0.,-1.44337567297406,1.27850268845987E-18));
#7549=CARTESIAN_POINT('',(0.,-0.721687836487032,-1.25));
#7550=CARTESIAN_POINT('',(0.,-0.721687836487032,-1.25));
#7551=CARTESIAN_POINT('',(0.,0.721687836487033,-1.25));
#7552=CARTESIAN_POINT('',(0.,0.721687836487033,-1.25));
#7553=CARTESIAN_POINT('',(0.,1.44337567297407,7.22223729145213E-31));
#7554=CARTESIAN_POINT('',(0.,1.44337567297407,7.22223729145213E-31));
#7555=CARTESIAN_POINT('',(0.,0.721687836487033,1.25));
#7556=CARTESIAN_POINT('Origin',(2.2,2.,0.));
#7557=CARTESIAN_POINT('Origin',(14.2,0.,0.));
#7558=CARTESIAN_POINT('Origin',(1.3,-1.44337567297406,1.27850268845987E-18));
#7559=CARTESIAN_POINT('',(1.3,-0.721687836487032,1.25));
#7560=CARTESIAN_POINT('',(1.3,-1.44337567297406,1.27850268845987E-18));
#7561=CARTESIAN_POINT('',(1.3,-1.44337567297406,1.27850268845987E-18));
#7562=CARTESIAN_POINT('',(1.3,-1.44337567297406,1.27850268845987E-18));
#7563=CARTESIAN_POINT('',(1.3,-1.44337567297406,1.27850268845987E-18));
#7564=CARTESIAN_POINT('',(1.3,-0.721687836487032,1.25));
#7565=CARTESIAN_POINT('Origin',(1.3,-0.721687836487032,-1.25));
#7566=CARTESIAN_POINT('',(1.3,-0.721687836487032,-1.25));
#7567=CARTESIAN_POINT('',(1.3,-0.721687836487032,-1.25));
#7568=CARTESIAN_POINT('',(1.3,-0.721687836487032,-1.25));
#7569=CARTESIAN_POINT('',(1.3,-0.721687836487032,-1.25));
#7570=CARTESIAN_POINT('Origin',(1.3,0.721687836487033,-1.25));
#7571=CARTESIAN_POINT('',(1.3,0.721687836487033,-1.25));
#7572=CARTESIAN_POINT('',(1.3,0.721687836487033,-1.25));
#7573=CARTESIAN_POINT('',(1.3,0.721687836487033,-1.25));
#7574=CARTESIAN_POINT('',(1.3,0.721687836487033,-1.25));
#7575=CARTESIAN_POINT('Origin',(1.3,1.44337567297407,7.22223729145213E-31));
#7576=CARTESIAN_POINT('',(1.3,1.44337567297407,7.22223729145213E-31));
#7577=CARTESIAN_POINT('',(1.3,1.44337567297407,7.22223729145213E-31));
#7578=CARTESIAN_POINT('',(1.3,1.44337567297407,7.22223729145213E-31));
#7579=CARTESIAN_POINT('',(1.3,1.44337567297407,7.22223729145213E-31));
#7580=CARTESIAN_POINT('Origin',(1.3,0.721687836487033,1.25));
#7581=CARTESIAN_POINT('',(1.3,0.721687836487033,1.25));
#7582=CARTESIAN_POINT('',(1.3,0.721687836487033,1.25));
#7583=CARTESIAN_POINT('',(1.3,0.721687836487033,1.25));
#7584=CARTESIAN_POINT('',(1.3,0.721687836487033,1.25));
#7585=CARTESIAN_POINT('Origin',(1.3,-0.721687836487032,1.25));
#7586=CARTESIAN_POINT('',(1.3,-0.721687836487032,1.25));
#7587=CARTESIAN_POINT('',(1.3,-0.721687836487032,1.25));
#7588=CARTESIAN_POINT('Origin',(1.3,-1.44337567297406,2.16840434497101E-16));
#7589=CARTESIAN_POINT('Origin',(1.3,-1.44337567297406,2.16840434497101E-16));
#7590=CARTESIAN_POINT('Origin',(1.3,-1.44337567297406,2.16840434497101E-16));
#7591=CARTESIAN_POINT('Origin',(1.3,-1.44337567297406,2.16840434497101E-16));
#7592=CARTESIAN_POINT('Origin',(1.3,-1.44337567297406,2.16840434497101E-16));
#7593=CARTESIAN_POINT('Origin',(1.3,-1.44337567297406,2.16840434497101E-16));
#7594=CARTESIAN_POINT('',(0.,0.,0.));
#7595=CARTESIAN_POINT('',(0.,0.,0.));
#7596=CARTESIAN_POINT('',(0.,0.,0.));
#7597=CARTESIAN_POINT('',(0.,0.,0.));
#7598=CARTESIAN_POINT('',(0.,0.,0.));
#7599=CARTESIAN_POINT('',(0.,0.,0.));
#7600=CARTESIAN_POINT('',(0.,0.,0.));
#7601=CARTESIAN_POINT('',(0.,0.,0.));
#7602=CARTESIAN_POINT('',(-6.66666666666667,17.2,20.5));
#7603=CARTESIAN_POINT('',(6.66666666666666,17.2,20.5));
#7604=CARTESIAN_POINT('',(6.66666666666666,17.2,-20.5));
#7605=CARTESIAN_POINT('',(-6.66666666666667,17.2,-20.5));
#7606=UNCERTAINTY_MEASURE_WITH_UNIT(LENGTH_MEASURE(0.01),#7628,
'DISTANCE_ACCURACY_VALUE',
'Maximum model space distance between geometric entities at asserted c
onnectivities');
#7607=UNCERTAINTY_MEASURE_WITH_UNIT(LENGTH_MEASURE(0.01),#7628,
'DISTANCE_ACCURACY_VALUE',
'Maximum model space distance between geometric entities at asserted c
onnectivities');
#7608=UNCERTAINTY_MEASURE_WITH_UNIT(LENGTH_MEASURE(0.01),#7628,
'DISTANCE_ACCURACY_VALUE',
'Maximum model space distance between geometric entities at asserted c
onnectivities');
#7609=UNCERTAINTY_MEASURE_WITH_UNIT(LENGTH_MEASURE(0.01),#7628,
'DISTANCE_ACCURACY_VALUE',
'Maximum model space distance between geometric entities at asserted c
onnectivities');
#7610=UNCERTAINTY_MEASURE_WITH_UNIT(LENGTH_MEASURE(0.01),#7628,
'DISTANCE_ACCURACY_VALUE',
'Maximum model space distance between geometric entities at asserted c
onnectivities');
#7611=UNCERTAINTY_MEASURE_WITH_UNIT(LENGTH_MEASURE(0.01),#7628,
'DISTANCE_ACCURACY_VALUE',
'Maximum model space distance between geometric entities at asserted c
onnectivities');
#7612=UNCERTAINTY_MEASURE_WITH_UNIT(LENGTH_MEASURE(0.01),#7628,
'DISTANCE_ACCURACY_VALUE',
'Maximum model space distance between geometric entities at asserted c
onnectivities');
#7613=UNCERTAINTY_MEASURE_WITH_UNIT(LENGTH_MEASURE(0.01),#7628,
'DISTANCE_ACCURACY_VALUE',
'Maximum model space distance between geometric entities at asserted c
onnectivities');
#7614=UNCERTAINTY_MEASURE_WITH_UNIT(LENGTH_MEASURE(0.01),#7628,
'DISTANCE_ACCURACY_VALUE',
'Maximum model space distance between geometric entities at asserted c
onnectivities');
#7615=UNCERTAINTY_MEASURE_WITH_UNIT(LENGTH_MEASURE(0.01),#7628,
'DISTANCE_ACCURACY_VALUE',
'Maximum model space distance between geometric entities at asserted c
onnectivities');
#7616=UNCERTAINTY_MEASURE_WITH_UNIT(LENGTH_MEASURE(0.01),#7628,
'DISTANCE_ACCURACY_VALUE',
'Maximum model space distance between geometric entities at asserted c
onnectivities');
#7617=(
GEOMETRIC_REPRESENTATION_CONTEXT(3)
GLOBAL_UNCERTAINTY_ASSIGNED_CONTEXT((#7606))
GLOBAL_UNIT_ASSIGNED_CONTEXT((#7628,#7630,#7631))
REPRESENTATION_CONTEXT('','3D')
);
#7618=(
GEOMETRIC_REPRESENTATION_CONTEXT(3)
GLOBAL_UNCERTAINTY_ASSIGNED_CONTEXT((#7607))
GLOBAL_UNIT_ASSIGNED_CONTEXT((#7628,#7630,#7631))
REPRESENTATION_CONTEXT('','3D')
);
#7619=(
GEOMETRIC_REPRESENTATION_CONTEXT(3)
GLOBAL_UNCERTAINTY_ASSIGNED_CONTEXT((#7608))
GLOBAL_UNIT_ASSIGNED_CONTEXT((#7628,#7630,#7631))
REPRESENTATION_CONTEXT('','3D')
);
#7620=(
GEOMETRIC_REPRESENTATION_CONTEXT(3)
GLOBAL_UNCERTAINTY_ASSIGNED_CONTEXT((#7609))
GLOBAL_UNIT_ASSIGNED_CONTEXT((#7628,#7630,#7631))
REPRESENTATION_CONTEXT('','3D')
);
#7621=(
GEOMETRIC_REPRESENTATION_CONTEXT(3)
GLOBAL_UNCERTAINTY_ASSIGNED_CONTEXT((#7610))
GLOBAL_UNIT_ASSIGNED_CONTEXT((#7628,#7630,#7631))
REPRESENTATION_CONTEXT('','3D')
);
#7622=(
GEOMETRIC_REPRESENTATION_CONTEXT(3)
GLOBAL_UNCERTAINTY_ASSIGNED_CONTEXT((#7611))
GLOBAL_UNIT_ASSIGNED_CONTEXT((#7628,#7630,#7631))
REPRESENTATION_CONTEXT('','3D')
);
#7623=(
GEOMETRIC_REPRESENTATION_CONTEXT(3)
GLOBAL_UNCERTAINTY_ASSIGNED_CONTEXT((#7612))
GLOBAL_UNIT_ASSIGNED_CONTEXT((#7628,#7630,#7631))
REPRESENTATION_CONTEXT('','3D')
);
#7624=(
GEOMETRIC_REPRESENTATION_CONTEXT(3)
GLOBAL_UNCERTAINTY_ASSIGNED_CONTEXT((#7613))
GLOBAL_UNIT_ASSIGNED_CONTEXT((#7628,#7630,#7631))
REPRESENTATION_CONTEXT('','3D')
);
#7625=(
GEOMETRIC_REPRESENTATION_CONTEXT(3)
GLOBAL_UNCERTAINTY_ASSIGNED_CONTEXT((#7614))
GLOBAL_UNIT_ASSIGNED_CONTEXT((#7628,#7630,#7631))
REPRESENTATION_CONTEXT('','3D')
);
#7626=(
GEOMETRIC_REPRESENTATION_CONTEXT(3)
GLOBAL_UNCERTAINTY_ASSIGNED_CONTEXT((#7615))
GLOBAL_UNIT_ASSIGNED_CONTEXT((#7628,#7630,#7631))
REPRESENTATION_CONTEXT('','3D')
);
#7627=(
GEOMETRIC_REPRESENTATION_CONTEXT(3)
GLOBAL_UNCERTAINTY_ASSIGNED_CONTEXT((#7616))
GLOBAL_UNIT_ASSIGNED_CONTEXT((#7628,#7630,#7631))
REPRESENTATION_CONTEXT('','3D')
);
#7628=(
LENGTH_UNIT()
NAMED_UNIT(*)
SI_UNIT(.MILLI.,.METRE.)
);
#7629=(
LENGTH_UNIT()
NAMED_UNIT(*)
SI_UNIT($,.METRE.)
);
#7630=(
NAMED_UNIT(*)
PLANE_ANGLE_UNIT()
SI_UNIT($,.RADIAN.)
);
#7631=(
NAMED_UNIT(*)
SI_UNIT($,.STERADIAN.)
SOLID_ANGLE_UNIT()
);
#7632=SHAPE_DEFINITION_REPRESENTATION(#7642,#7664);
#7633=SHAPE_DEFINITION_REPRESENTATION(#7643,#7665);
#7634=SHAPE_DEFINITION_REPRESENTATION(#7644,#7666);
#7635=SHAPE_DEFINITION_REPRESENTATION(#7645,#7667);
#7636=SHAPE_DEFINITION_REPRESENTATION(#7646,#7668);
#7637=SHAPE_DEFINITION_REPRESENTATION(#7647,#7669);
#7638=SHAPE_DEFINITION_REPRESENTATION(#7648,#7670);
#7639=SHAPE_DEFINITION_REPRESENTATION(#7649,#7671);
#7640=SHAPE_DEFINITION_REPRESENTATION(#7650,#7672);
#7641=SHAPE_DEFINITION_REPRESENTATION(#7651,#7673);
#7642=PRODUCT_DEFINITION_SHAPE('',$,#7675);
#7643=PRODUCT_DEFINITION_SHAPE('',$,#7676);
#7644=PRODUCT_DEFINITION_SHAPE('',$,#7677);
#7645=PRODUCT_DEFINITION_SHAPE('',$,#7678);
#7646=PRODUCT_DEFINITION_SHAPE('',$,#7679);
#7647=PRODUCT_DEFINITION_SHAPE('',$,#7680);
#7648=PRODUCT_DEFINITION_SHAPE('',$,#7681);
#7649=PRODUCT_DEFINITION_SHAPE('',$,#7682);
#7650=PRODUCT_DEFINITION_SHAPE('',$,#7683);
#7651=PRODUCT_DEFINITION_SHAPE('',$,#7684);
#7652=PRODUCT_DEFINITION_SHAPE($,$,#47);
#7653=PRODUCT_DEFINITION_SHAPE($,$,#48);
#7654=PRODUCT_DEFINITION_SHAPE($,$,#49);
#7655=PRODUCT_DEFINITION_SHAPE($,$,#50);
#7656=PRODUCT_DEFINITION_SHAPE($,$,#51);
#7657=PRODUCT_DEFINITION_SHAPE($,$,#52);
#7658=PRODUCT_DEFINITION_SHAPE($,$,#53);
#7659=PRODUCT_DEFINITION_SHAPE($,$,#54);
#7660=PRODUCT_DEFINITION_SHAPE($,$,#55);
#7661=PRODUCT_DEFINITION_SHAPE($,$,#56);
#7662=PRODUCT_DEFINITION_SHAPE($,$,#57);
#7663=PRODUCT_DEFINITION_SHAPE($,$,#58);
#7664=SHAPE_REPRESENTATION('',(#2534,#2852,#2853,#2854,#2855,#2856,#2857,
#2858,#2859,#2860,#2861,#2862,#2863),#7617);
#7665=SHAPE_REPRESENTATION('',(#2535),#7618);
#7666=SHAPE_REPRESENTATION('',(#2572),#7619);
#7667=SHAPE_REPRESENTATION('',(#2590),#7620);
#7668=SHAPE_REPRESENTATION('',(#2600),#7621);
#7669=SHAPE_REPRESENTATION('',(#2608),#7622);
#7670=SHAPE_REPRESENTATION('',(#2630),#7623);
#7671=SHAPE_REPRESENTATION('',(#2645),#7624);
#7672=SHAPE_REPRESENTATION('',(#2776),#7625);
#7673=SHAPE_REPRESENTATION('',(#2816),#7626);
#7674=PRODUCT_DEFINITION_CONTEXT('part definition',#7706,'design');
#7675=PRODUCT_DEFINITION('Compact Solenoid Valve',
'TAS-003',#7685,#7674);
#7676=PRODUCT_DEFINITION('Brass Valve Body','Brass Valve Body',#7686,#7674);
#7677=PRODUCT_DEFINITION('Plunger','Plunger',#7687,#7674);
#7678=PRODUCT_DEFINITION('seal','seal',#7688,#7674);
#7679=PRODUCT_DEFINITION('Return Spring','Return Spring',#7689,#7674);
#7680=PRODUCT_DEFINITION('valve seat','valve seat',#7690,#7674);
#7681=PRODUCT_DEFINITION('armature','armature',#7691,#7674);
#7682=PRODUCT_DEFINITION('coil','coil',#7692,#7674);
#7683=PRODUCT_DEFINITION('Coil Housing','Coil Housing',#7693,#7674);
#7684=PRODUCT_DEFINITION(
'socket button head screw_iso_ISO 7380 - M4 x 12 - 12N',
'socket button head screw_iso_ISO 7380 - M4 x 12 - 12N',#7694,#7674);
#7685=PRODUCT_DEFINITION_FORMATION('',$,#7708);
#7686=PRODUCT_DEFINITION_FORMATION('',$,#7709);
#7687=PRODUCT_DEFINITION_FORMATION('',$,#7710);
#7688=PRODUCT_DEFINITION_FORMATION('',$,#7711);
#7689=PRODUCT_DEFINITION_FORMATION('',$,#7712);
#7690=PRODUCT_DEFINITION_FORMATION('',$,#7713);
#7691=PRODUCT_DEFINITION_FORMATION('',$,#7714);
#7692=PRODUCT_DEFINITION_FORMATION('',$,#7715);
#7693=PRODUCT_DEFINITION_FORMATION('',$,#7716);
#7694=PRODUCT_DEFINITION_FORMATION('',$,#7717);
#7695=PRODUCT_RELATED_PRODUCT_CATEGORY('TAS-003',
'TAS-003',(#7708));
#7696=PRODUCT_RELATED_PRODUCT_CATEGORY('Brass Valve Body',
'Brass Valve Body',(#7709));
#7697=PRODUCT_RELATED_PRODUCT_CATEGORY('Plunger','Plunger',(#7710));
#7698=PRODUCT_RELATED_PRODUCT_CATEGORY('seal','seal',(#7711));
#7699=PRODUCT_RELATED_PRODUCT_CATEGORY('Return Spring','Return Spring',
(#7712));
#7700=PRODUCT_RELATED_PRODUCT_CATEGORY('valve seat','valve seat',(#7713));
#7701=PRODUCT_RELATED_PRODUCT_CATEGORY('armature','armature',(#7714));
#7702=PRODUCT_RELATED_PRODUCT_CATEGORY('coil','coil',(#7715));
#7703=PRODUCT_RELATED_PRODUCT_CATEGORY('Coil Housing','Coil Housing',(#7716));
#7704=PRODUCT_RELATED_PRODUCT_CATEGORY(
'socket button head screw_iso_ISO 7380 - M4 x 12 - 12N',
'socket button head screw_iso_ISO 7380 - M4 x 12 - 12N',(#7717));
#7705=APPLICATION_PROTOCOL_DEFINITION('international standard',
'automotive_design',2009,#7706);
#7706=APPLICATION_CONTEXT(
'Core Data for Automotive Mechanical Design Process');
#7707=PRODUCT_CONTEXT('part definition',#7706,'mechanical');
#7708=PRODUCT('Compact Solenoid Valve','TAS-003',
'STEP AP214',(#7707));
#7709=PRODUCT('Brass Valve Body','Brass Valve Body',$,(#7707));
#7710=PRODUCT('Plunger','Plunger',$,(#7707));
#7711=PRODUCT('seal','seal',$,(#7707));
#7712=PRODUCT('Return Spring','Return Spring',$,(#7707));
#7713=PRODUCT('valve seat','valve seat',$,(#7707));
#7714=PRODUCT('armature','armature',$,(#7707));
#7715=PRODUCT('coil','coil',$,(#7707));
#7716=PRODUCT('Coil Housing','Coil Housing',$,(#7707));
#7717=PRODUCT('socket button head screw_iso_ISO 7380 - M4 x 12 - 12N',
'socket button head screw_iso_ISO 7380 - M4 x 12 - 12N',$,(#7707));
#7718=PRESENTATION_STYLE_ASSIGNMENT((#7724));
#7719=PRESENTATION_STYLE_ASSIGNMENT((#7725));
#7720=PRESENTATION_STYLE_ASSIGNMENT((#7726));
#7721=PRESENTATION_STYLE_ASSIGNMENT((#7727));
#7722=PRESENTATION_STYLE_ASSIGNMENT((#7728));
#7723=PRESENTATION_STYLE_ASSIGNMENT((#7729));
#7724=SURFACE_STYLE_USAGE(.BOTH.,#7730);
#7725=SURFACE_STYLE_USAGE(.BOTH.,#7731);
#7726=SURFACE_STYLE_USAGE(.BOTH.,#7732);
#7727=SURFACE_STYLE_USAGE(.BOTH.,#7733);
#7728=SURFACE_STYLE_USAGE(.BOTH.,#7734);
#7729=SURFACE_STYLE_USAGE(.BOTH.,#7735);
#7730=SURFACE_SIDE_STYLE('',(#7736));
#7731=SURFACE_SIDE_STYLE('',(#7737));
#7732=SURFACE_SIDE_STYLE('',(#7738));
#7733=SURFACE_SIDE_STYLE('',(#7739));
#7734=SURFACE_SIDE_STYLE('',(#7740));
#7735=SURFACE_SIDE_STYLE('',(#7741));
#7736=SURFACE_STYLE_FILL_AREA(#7742);
#7737=SURFACE_STYLE_FILL_AREA(#7743);
#7738=SURFACE_STYLE_FILL_AREA(#7744);
#7739=SURFACE_STYLE_FILL_AREA(#7745);
#7740=SURFACE_STYLE_FILL_AREA(#7746);
#7741=SURFACE_STYLE_FILL_AREA(#7747);
#7742=FILL_AREA_STYLE('Steel - Satin',(#7748));
#7743=FILL_AREA_STYLE('Opaque(20,51,87)',(#7749));
#7744=FILL_AREA_STYLE('Opaque(227,224,212)',(#7750));
#7745=FILL_AREA_STYLE('Opaque(31,36,43)',(#7751));
#7746=FILL_AREA_STYLE('Opaque(122,133,145)',(#7752));
#7747=FILL_AREA_STYLE('Opaque(97,158,199)',(#7753));
#7748=FILL_AREA_STYLE_COLOUR('Steel - Satin',#7754);
#7749=FILL_AREA_STYLE_COLOUR('Opaque(20,51,87)',#7755);
#7750=FILL_AREA_STYLE_COLOUR('Opaque(227,224,212)',#7756);
#7751=FILL_AREA_STYLE_COLOUR('Opaque(31,36,43)',#7757);
#7752=FILL_AREA_STYLE_COLOUR('Opaque(122,133,145)',#7758);
#7753=FILL_AREA_STYLE_COLOUR('Opaque(97,158,199)',#7759);
#7754=COLOUR_RGB('Steel - Satin',0.627450980392157,0.627450980392157,0.627450980392157);
#7755=COLOUR_RGB('Opaque(20,51,87)',0.0784313725490196,0.2,0.341176470588235);
#7756=COLOUR_RGB('Opaque(227,224,212)',0.890196078431372,0.87843137254902,
0.831372549019608);
#7757=COLOUR_RGB('Opaque(31,36,43)',0.12156862745098,0.141176470588235,
0.168627450980392);
#7758=COLOUR_RGB('Opaque(122,133,145)',0.47843137254902,0.52156862745098,
0.568627450980392);
#7759=COLOUR_RGB('Opaque(97,158,199)',0.380392156862745,0.619607843137255,
0.780392156862745);
ENDSEC;
END-ISO-10303-21;
